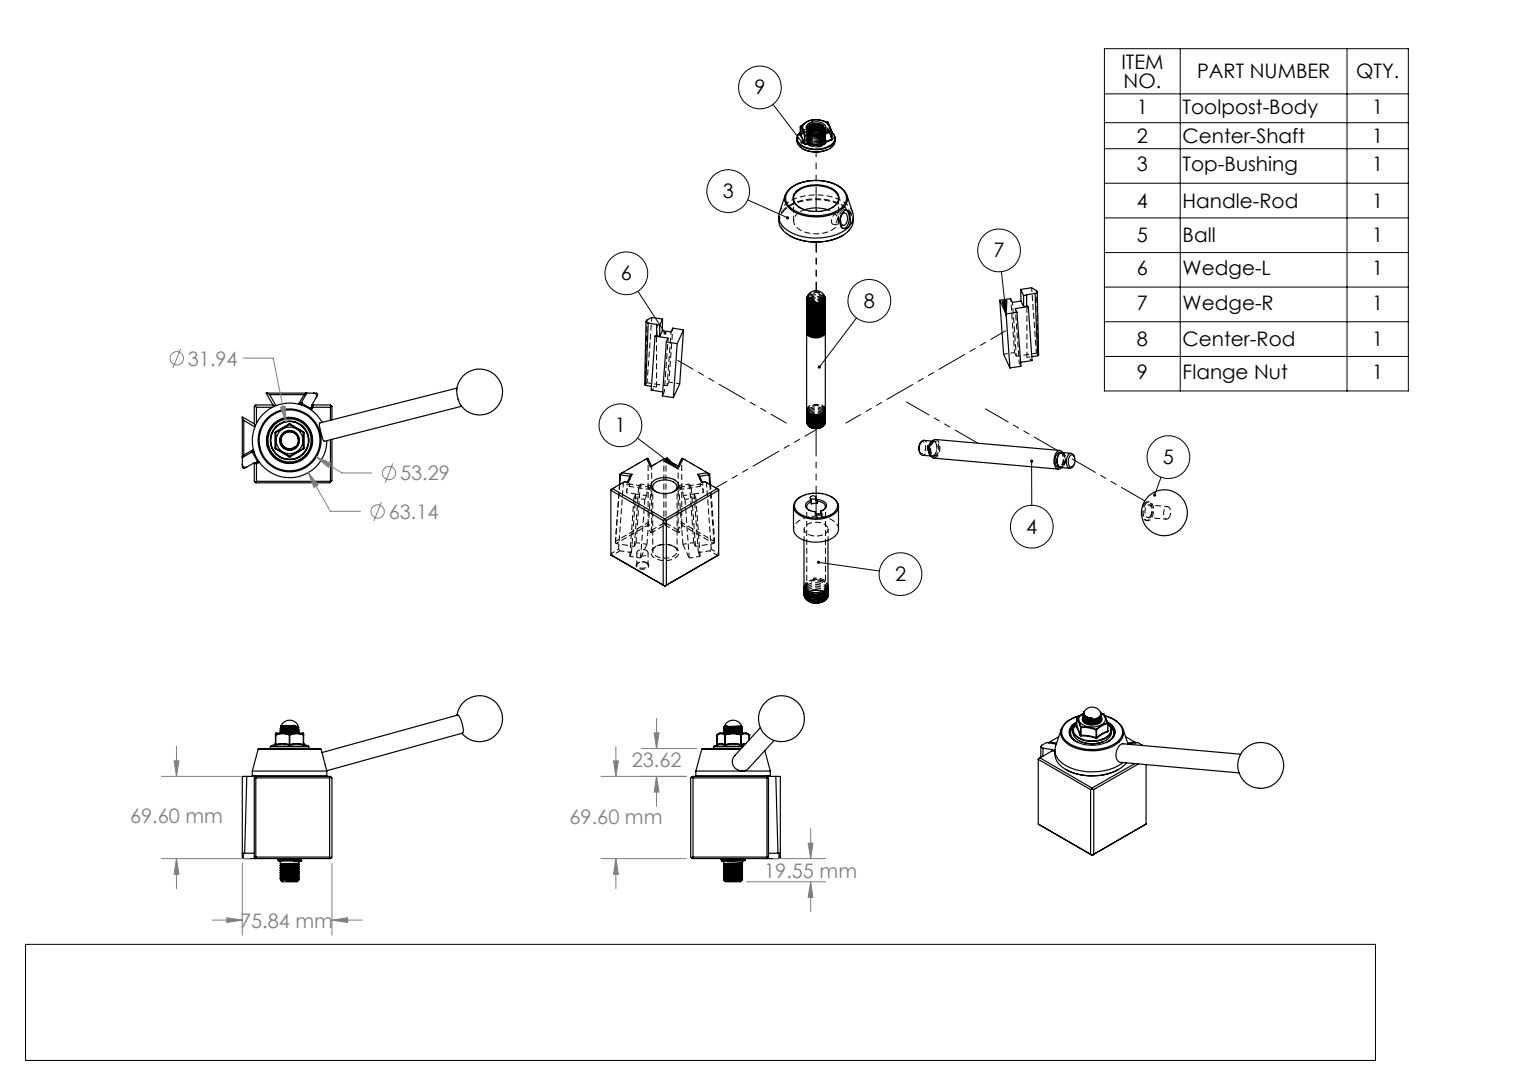
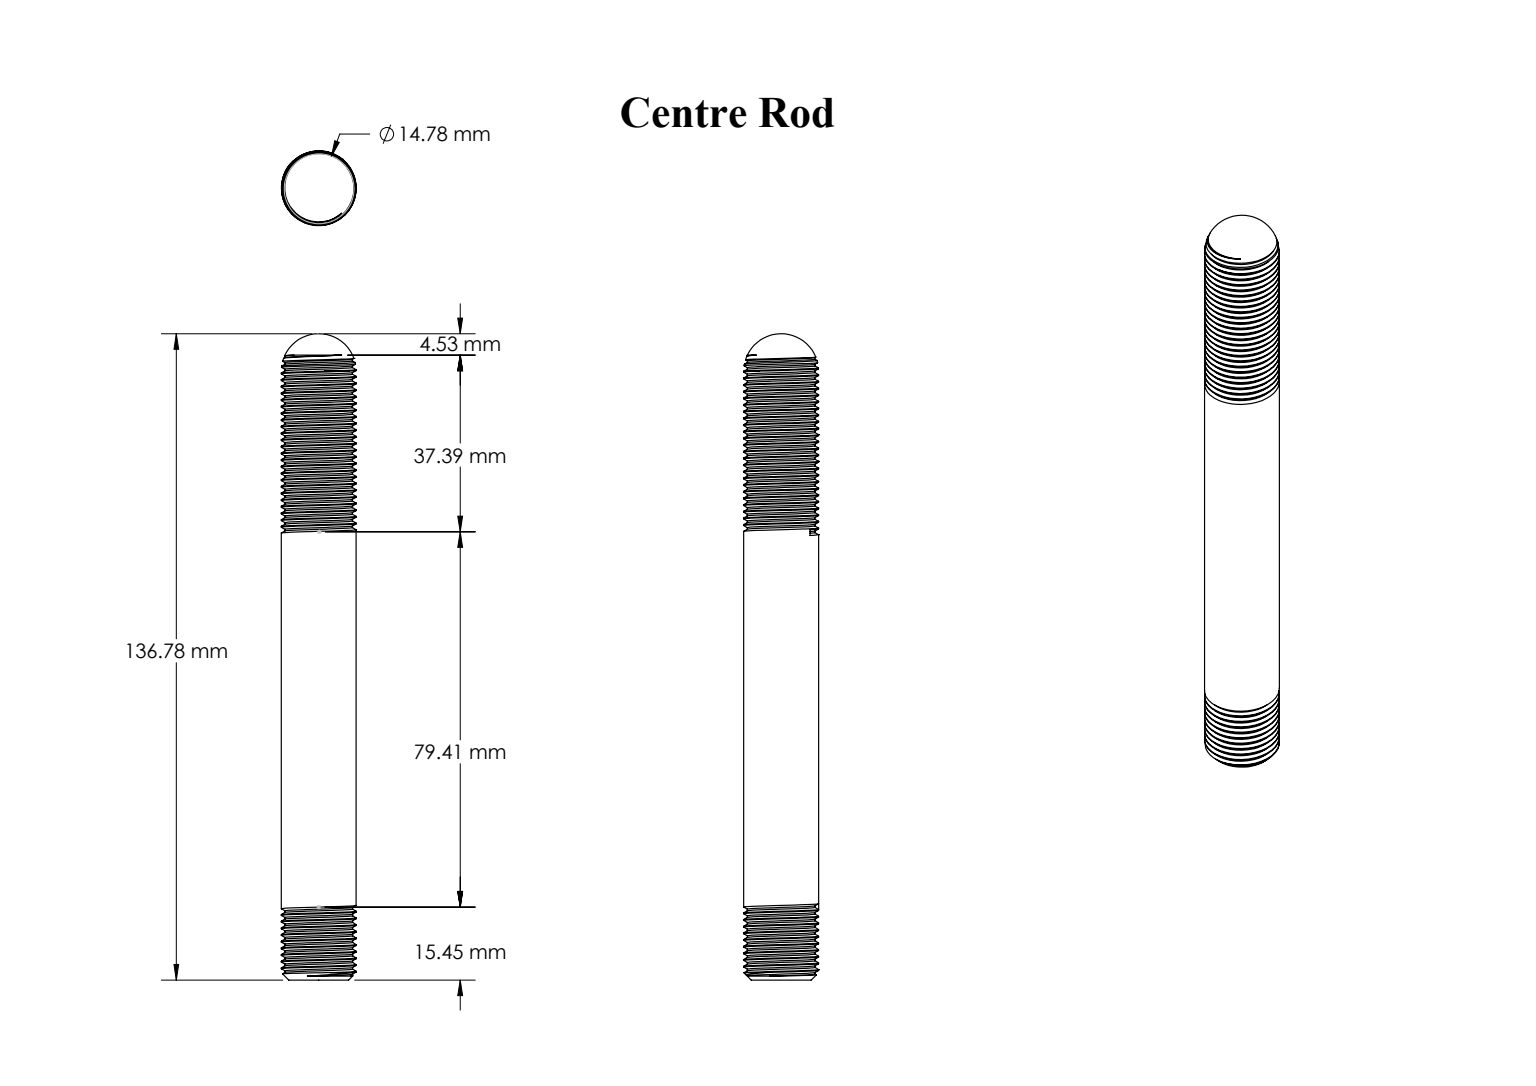
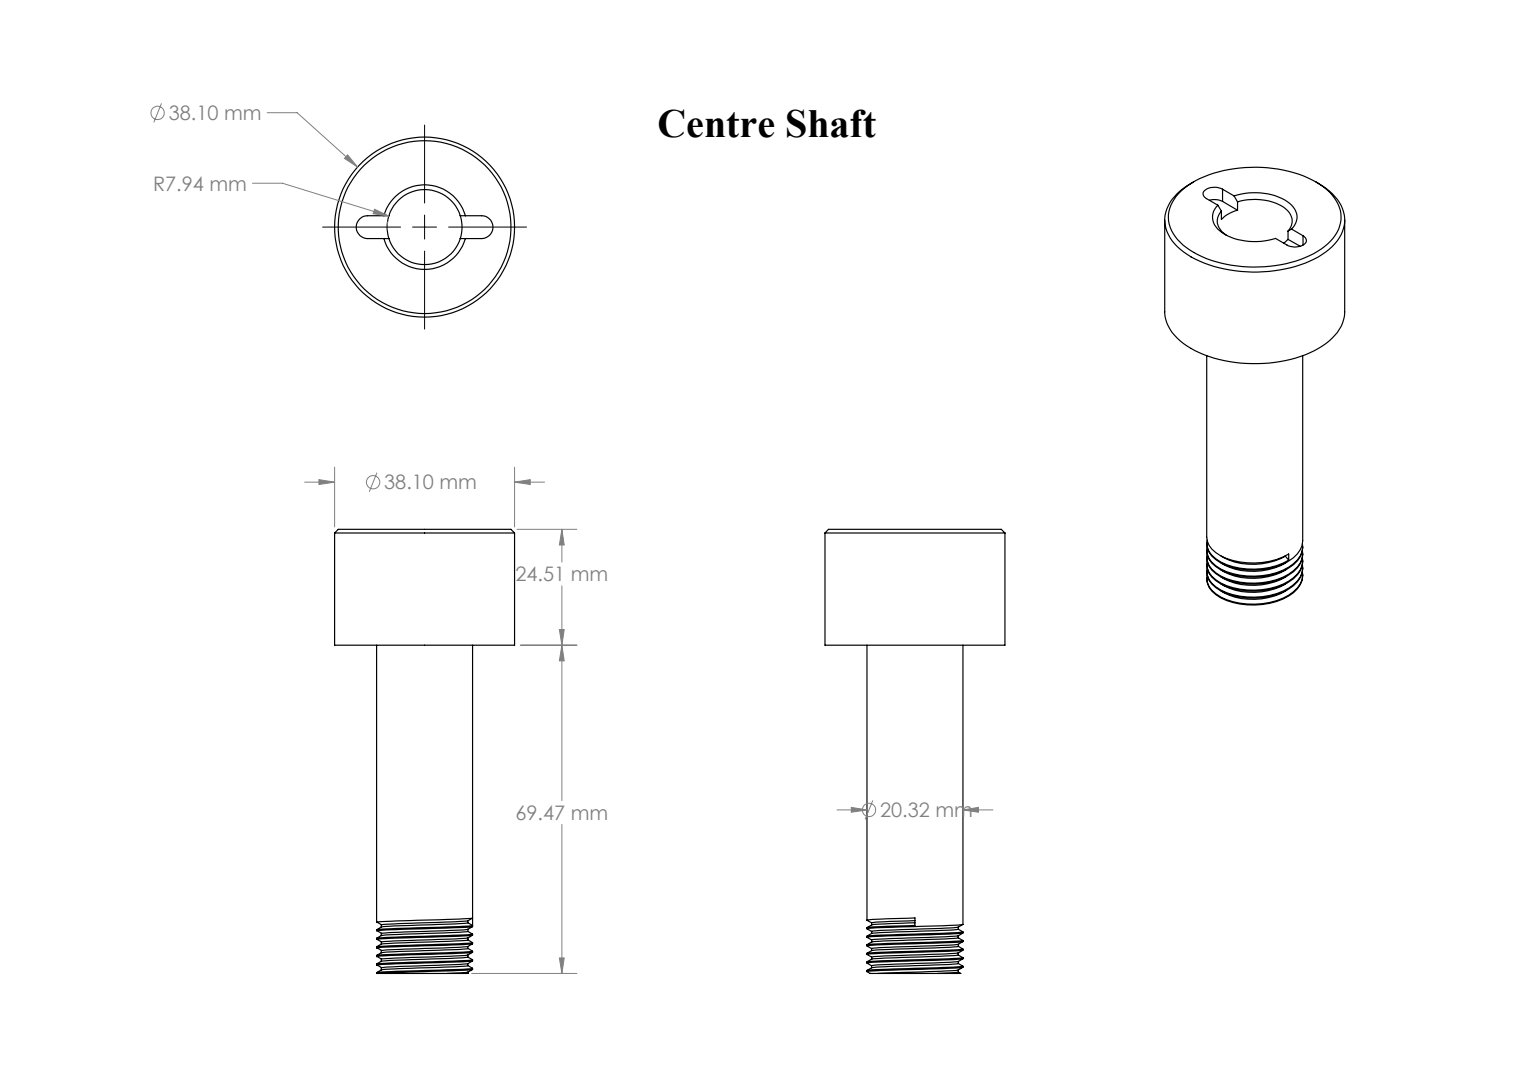
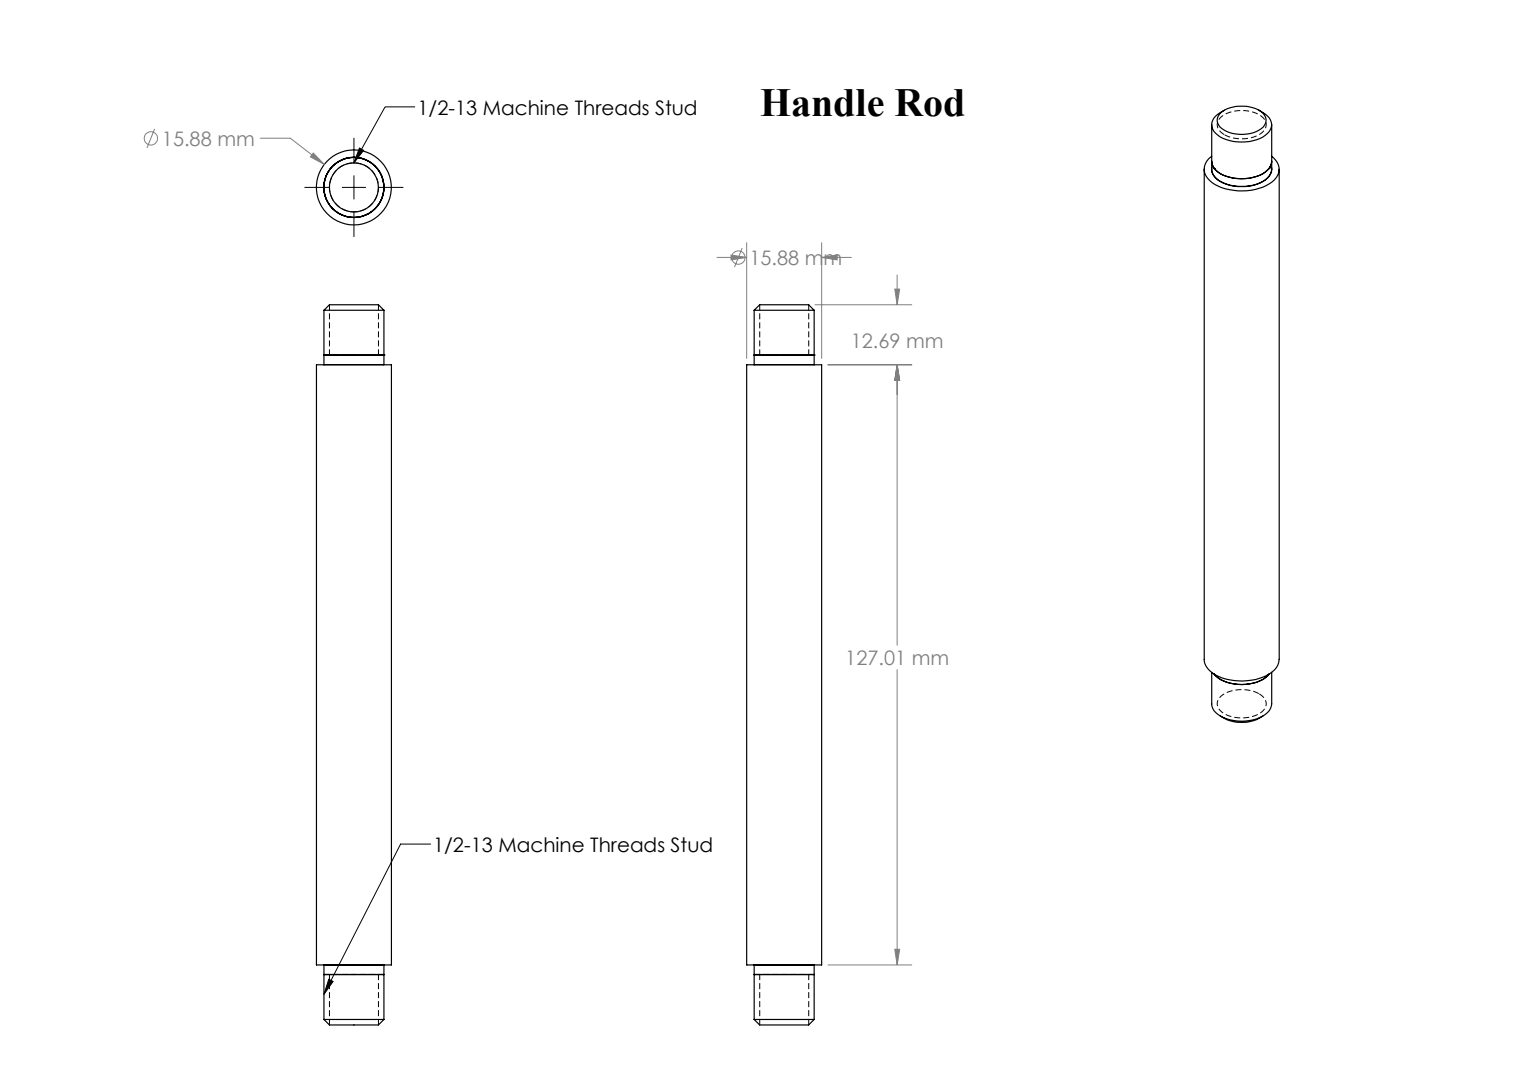
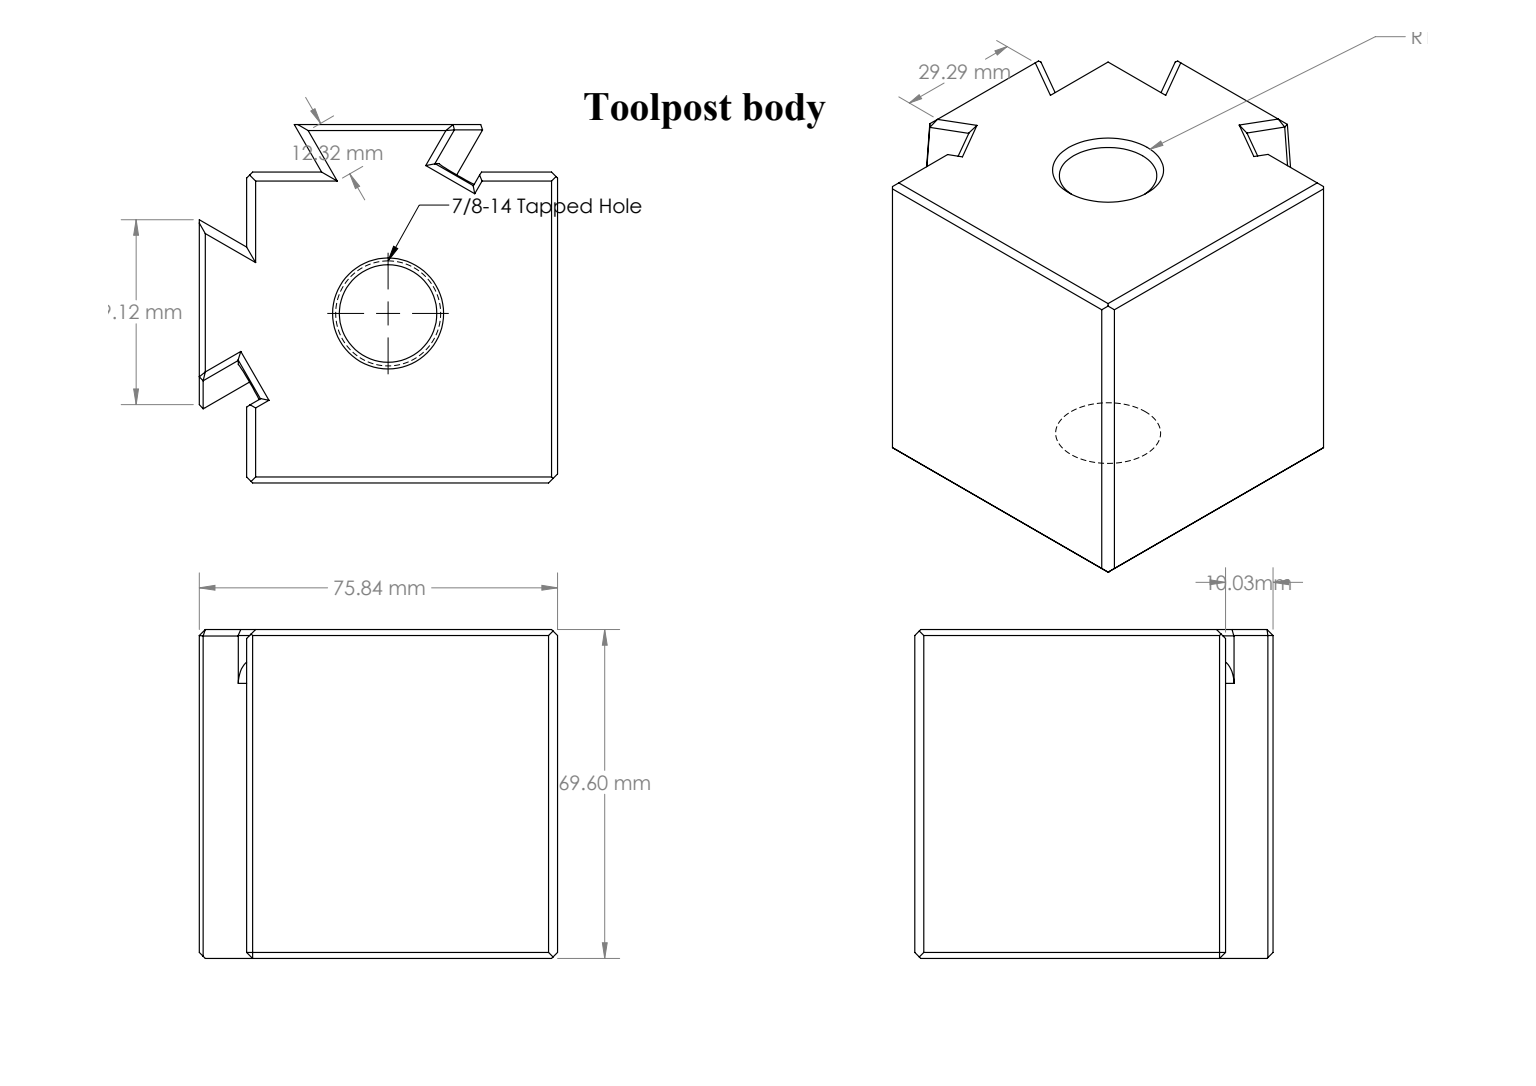
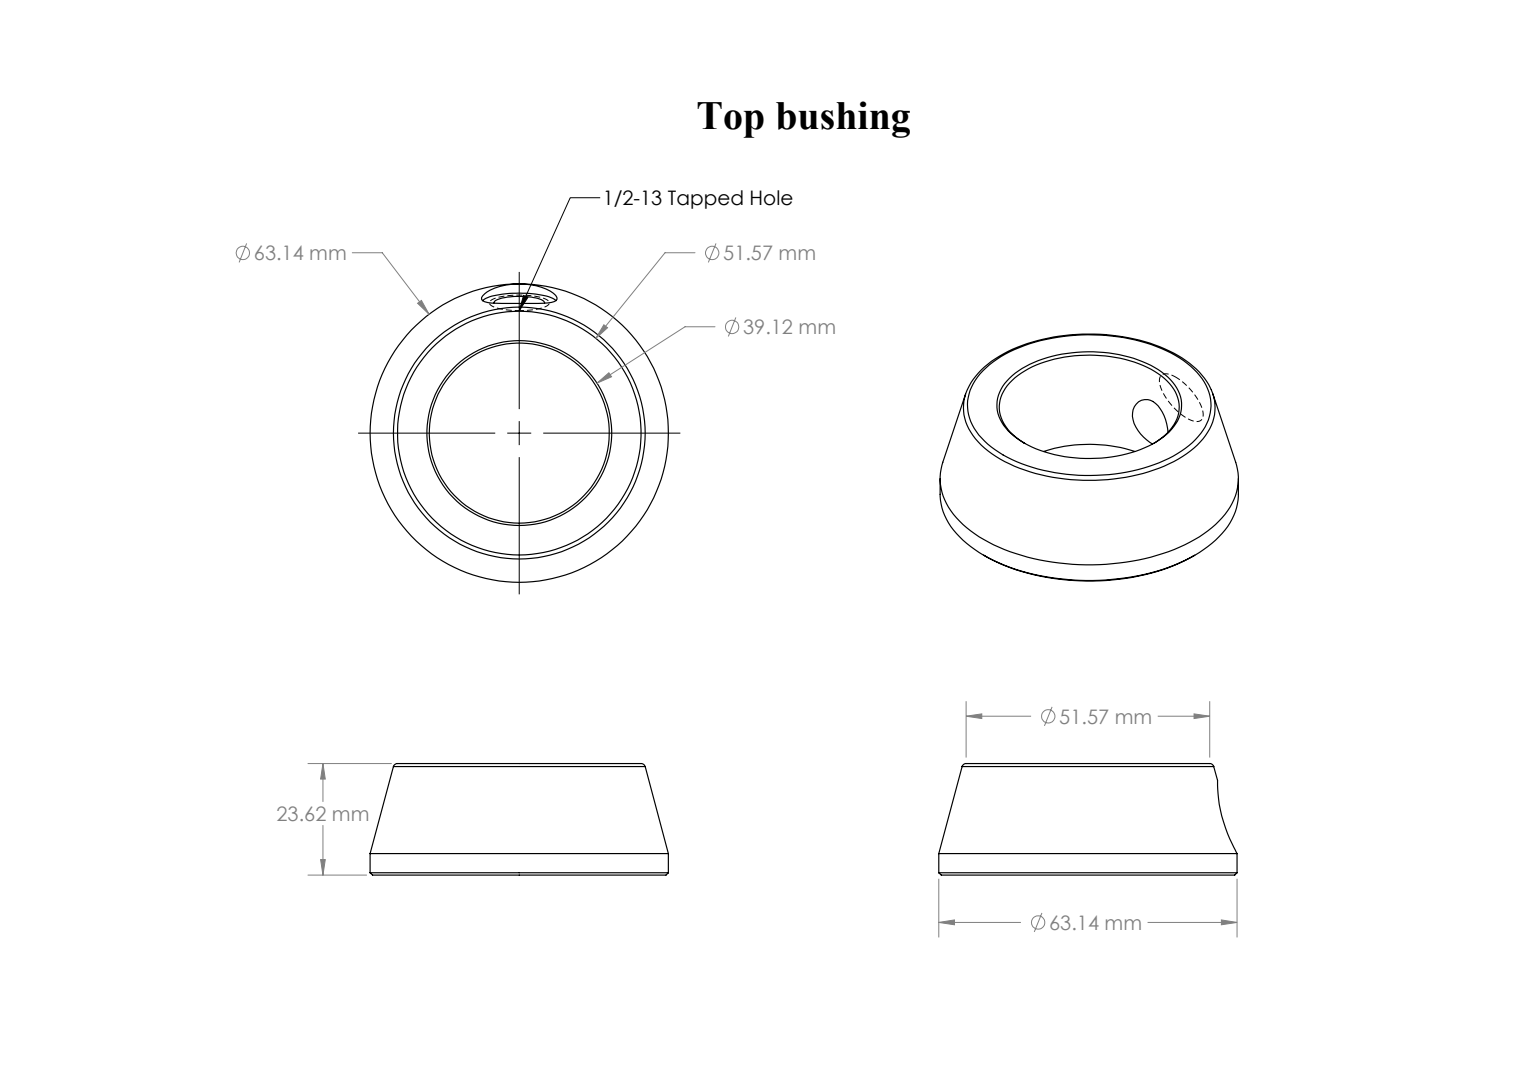
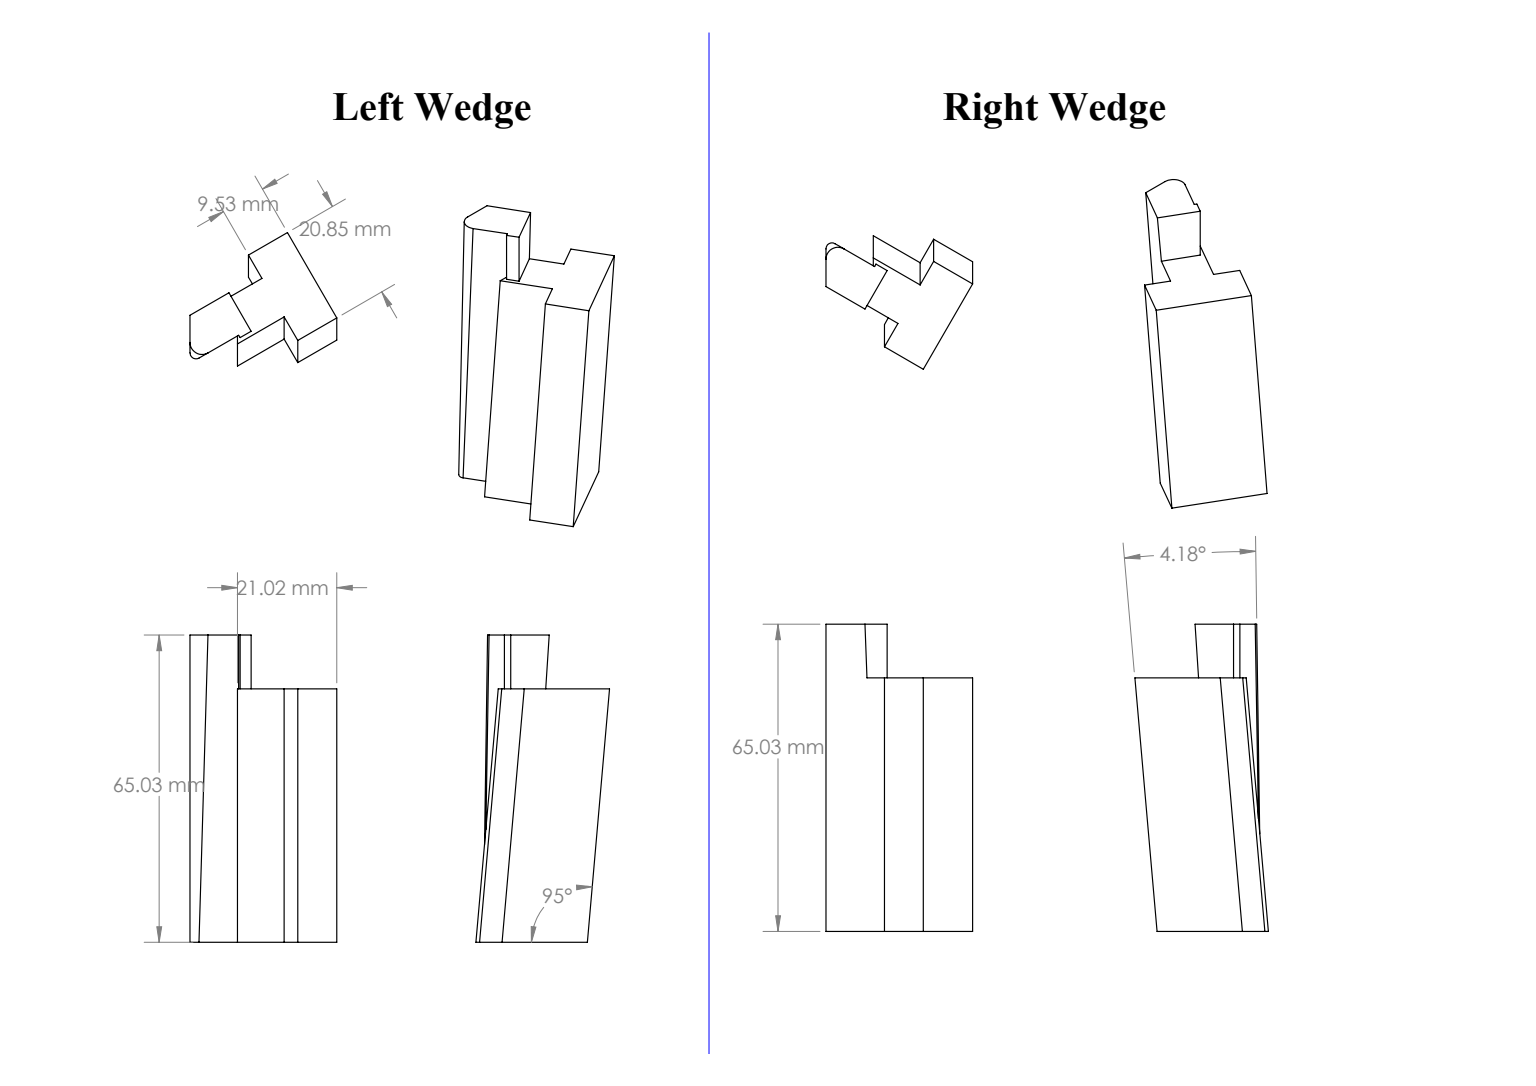
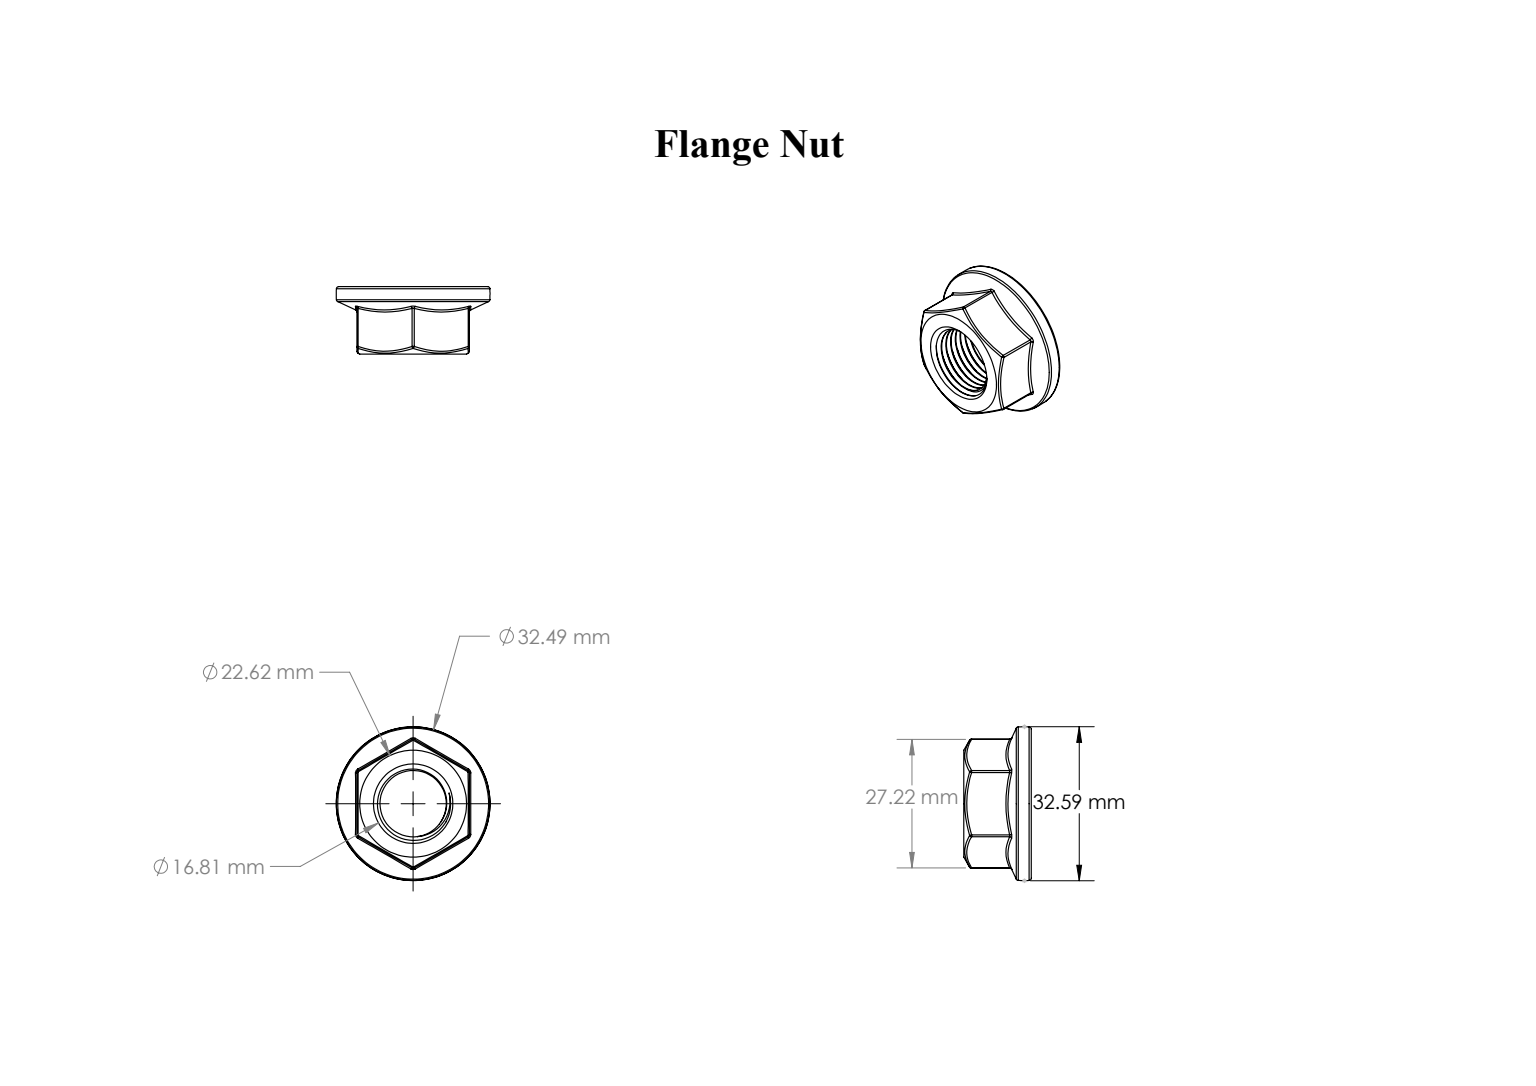
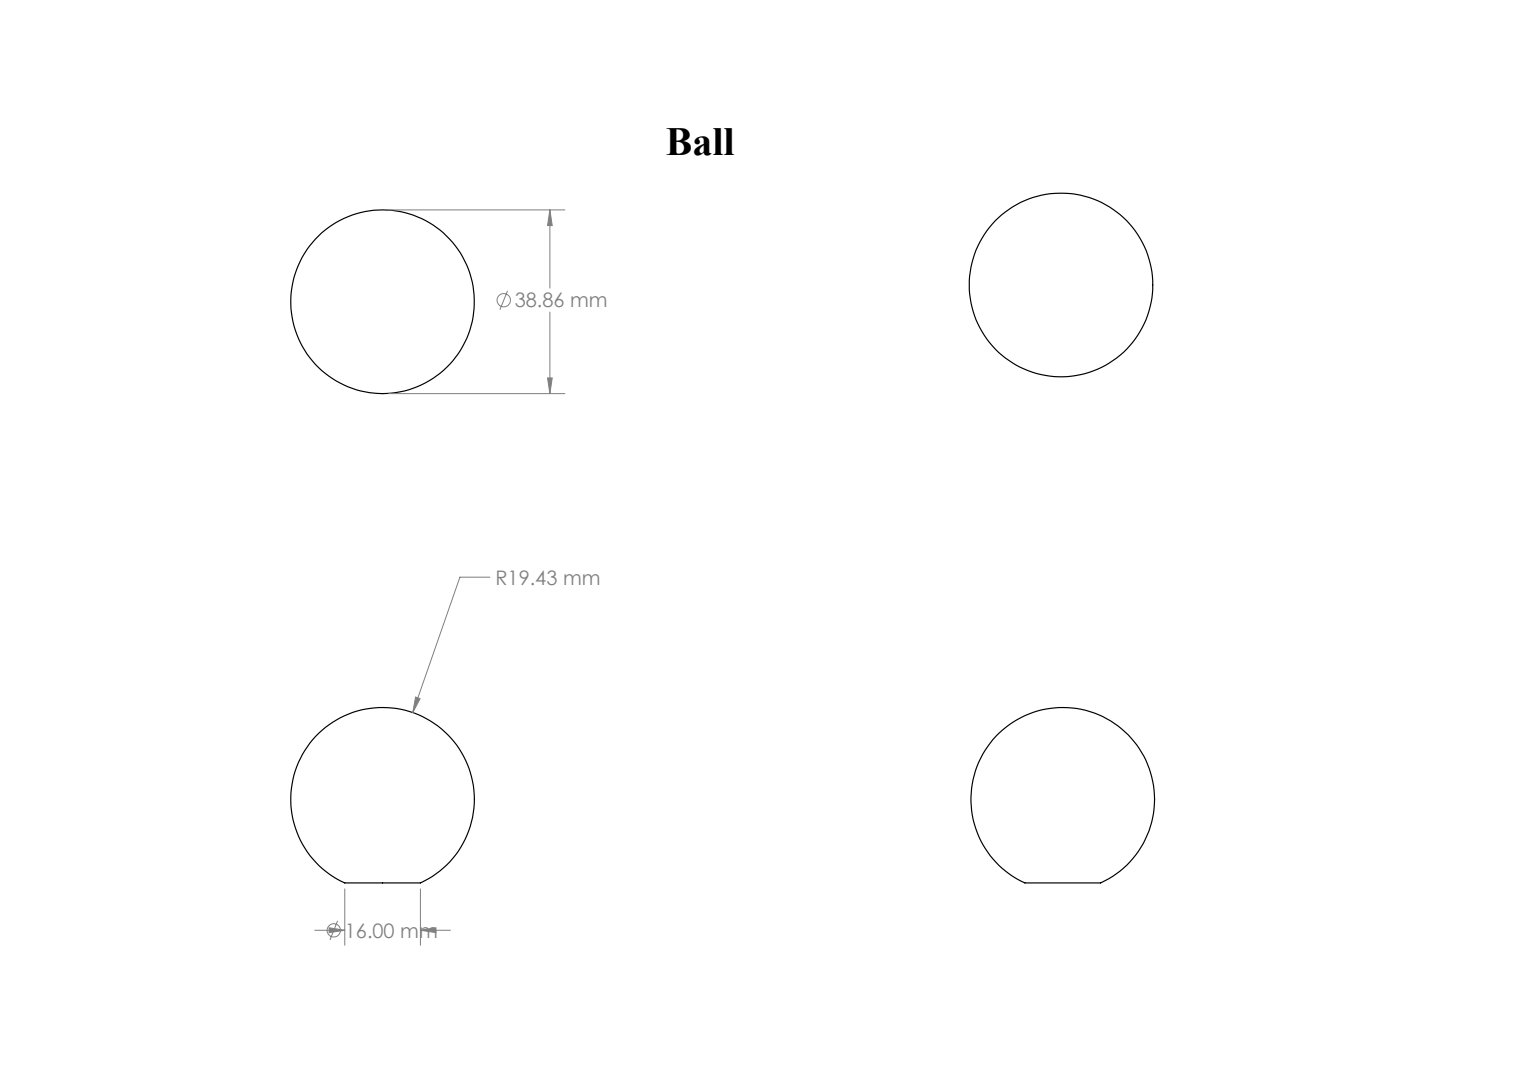
ISO-10303-21;
HEADER;
FILE_DESCRIPTION (('STEP AP203'),
    '1' );
FILE_NAME ('MAS-409',
    '2026-10-07T20:09:13',
    ( '' ),
    ( '' ),
    'SwSTEP 2.0',
    'SolidWorks 2024',
    '' );
FILE_SCHEMA (( 'AUTOMOTIVE_DESIGN' ));
ENDSEC;

DATA;
#1 = DIRECTION ( 'NONE',  ( 1.000000000000000000, 7.888609052210118054E-31, 7.888609052210118054E-31 ) ) ;
#2 = CARTESIAN_POINT ( 'NONE',  ( 0.2472135954999579721, 0.2589285712334865597, -0.3402603233408160732 ) ) ;
#3 = CARTESIAN_POINT ( 'NONE',  ( 1.910449006669871087E-17, 0.1986111111111107386, -0.3119999999999999996 ) ) ;
#4 = CARTESIAN_POINT ( 'NONE',  ( 0.1993543840281267465, 4.595916666742532186, 0.1993543840281266633 ) ) ;
#5 = DATE_AND_TIME ( #15379, #11143 ) ;
#6 = CARTESIAN_POINT ( 'NONE',  ( -0.3119999999999999996, 4.772999999999998799, 0.000000000000000000 ) ) ;
#7 = CARTESIAN_POINT ( 'NONE',  ( 0.8119709581221709049, 2.978485840173427324, -1.588368860739399313 ) ) ;
#8 = CARTESIAN_POINT ( 'NONE',  ( -0.1167790944451422702, 0.4555555554796890116, -0.2819296736111110424 ) ) ;
#9 = ORIENTED_EDGE ( 'NONE', *, *, #4852, .T. ) ;
#10 = EDGE_LOOP ( 'NONE', ( #22952, #23835 ) ) ;
#11 = CARTESIAN_POINT ( 'NONE',  ( -0.1993543840281266633, 0.1256944443685777957, -0.1993543840281266910 ) ) ;
#12 = CARTESIAN_POINT ( 'NONE',  ( 0.4200000000000001510, 0.05000000000000028727, -2.565999999999999837 ) ) ;
#13 = CARTESIAN_POINT ( 'NONE',  ( 0.000000000000000000, 5.384999999999999787, 0.000000000000000000 ) ) ;
#14 = CARTESIAN_POINT ( 'NONE',  ( -0.3236067977499789694, 0.1428571428571428215, -0.2351141009169893104 ) ) ;
#15 = CARTESIAN_POINT ( 'NONE',  ( 0.3155070326520292845, -5.795770164686806123E-17, 0.03451388888889012074 ) ) ;
#16 = CARTESIAN_POINT ( 'NONE',  ( 0.3124999999999999445, -0.1294417382415923856, 0.03625000000000165590 ) ) ;
#17 = AXIS2_PLACEMENT_3D ( 'NONE', #19179, #8074, #22716 ) ;
#18 = FACE_OUTER_BOUND ( 'NONE', #649, .T. ) ;
#19 = CARTESIAN_POINT ( 'NONE',  ( -0.1167790944451422702, 0.2194444443685778234, -0.2819296736111110979 ) ) ;
#20 = CARTESIAN_POINT ( 'NONE',  ( 0.1993543840281266355, 0.02847222214635558926, 0.1993543840281267465 ) ) ;
#21 = VECTOR ( 'NONE', #10740, 39.37007874015748143 ) ;
#22 = CARTESIAN_POINT ( 'NONE',  ( -1.726321361862525858E-17, 4.575083333409199149, -0.2819296736111110979 ) ) ;
#23 = CARTESIAN_POINT ( 'NONE',  ( -0.4000000000000000222, 0.06964285694777234970, -4.898587196589413075E-17 ) ) ;
#24 = CARTESIAN_POINT ( 'NONE',  ( 0.1554777997599670336, -3.800488706749824749E-17, -0.3394405886668848682 ) ) ;
#25 = CARTESIAN_POINT ( 'NONE',  ( 0.1993543840281266633, 5.179250000075866112, -0.1993543840281266910 ) ) ;
#26 = CARTESIAN_POINT ( 'NONE',  ( -0.2819296736111110979, 4.349388888964754507, -0.1167790944451422980 ) ) ;
#27 = CARTESIAN_POINT ( 'NONE',  ( 0.3137165877996647145, 3.752159157235426701, 0.001669988021508127815 ) ) ;
#28 = CARTESIAN_POINT ( 'NONE',  ( -0.1899274842524383000, 0.4207833852643000361, 0.4343212420608417168 ) ) ;
#29 = DIRECTION ( 'NONE',  ( -0.000000000000000000, -1.000000000000000000, -0.000000000000000000 ) ) ;
#30 = ADVANCED_FACE ( 'NONE', ( #19654 ), #17708, .T. ) ;
#31 = CARTESIAN_POINT ( 'NONE',  ( -0.1292346314604057023, 4.123694444596177178, 0.3119999999999998885 ) ) ;
#32 = CARTESIAN_POINT ( 'NONE',  ( -0.2819296736111110979, 4.533416666742532186, 0.000000000000000000 ) ) ;
#33 = DIRECTION ( 'NONE',  ( 0.000000000000000000, 0.7071067811865497932, 0.7071067811865452413 ) ) ;
#34 = EDGE_CURVE ( 'NONE', #12593, #3702, #6524, .T. ) ;
#35 = CARTESIAN_POINT ( 'NONE',  ( -0.3616234456863465230, 3.514980167629567998, 2.635972749958888528 ) ) ;
#36 = ORIENTED_EDGE ( 'NONE', *, *, #677, .F. ) ;
#37 = VECTOR ( 'NONE', #16324, 39.37007874015748143 ) ;
#38 = ORIENTED_EDGE ( 'NONE', *, *, #20394, .F. ) ;
#39 = PERSON_AND_ORGANIZATION_ROLE ( 'classification_officer' ) ;
#40 = FACE_OUTER_BOUND ( 'NONE', #1469, .T. ) ;
#41 = CARTESIAN_POINT ( 'NONE',  ( 0.4208308994021709992, -0.2864083541825031554, 0.4065068718547069082 ) ) ;
#42 = DIRECTION ( 'NONE',  ( -0.000000000000000000, 0.000000000000000000, 1.000000000000000000 ) ) ;
#43 = EDGE_LOOP ( 'NONE', ( #17199, #17644, #7483, #15061 ) ) ;
#44 = CARTESIAN_POINT ( 'NONE',  ( -0.3119999999999999996, 0.4277777776260448528, -3.820898013339742174E-17 ) ) ;
#45 = VERTEX_POINT ( 'NONE', #6974 ) ;
#46 = DIRECTION ( 'NONE',  ( 0.000000000000000000, 0.000000000000000000, -1.000000000000000000 ) ) ;
#47 = CARTESIAN_POINT ( 'NONE',  ( -0.3140464948364212194, 3.723602166599303764, -0.02909203108594766995 ) ) ;
#48 = CARTESIAN_POINT ( 'NONE',  ( -0.1116596296178200276, 0.04374999990245760639, 0.3436530038418508792 ) ) ;
#49 = CARTESIAN_POINT ( 'NONE',  ( 0.1916168258699956772, 3.966268988801258555, 0.2495847059250467792 ) ) ;
#50 = ORIENTED_EDGE ( 'NONE', *, *, #21102, .T. ) ;
#51 = CARTESIAN_POINT ( 'NONE',  ( 0.3613381517857143232, 0.08660714275960043618, -0.1174058825155740587 ) ) ;
#52 = ORIENTED_EDGE ( 'NONE', *, *, #22032, .T. ) ;
#53 = CARTESIAN_POINT ( 'NONE',  ( 0.4500000000000003442, 0.2598076211353318454, 0.3779506566538942125 ) ) ;
#54 = CARTESIAN_POINT ( 'NONE',  ( -0.2764156081756484196, 1.692557448933383907E-17, 0.2550000000000032241 ) ) ;
#55 = CARTESIAN_POINT ( 'NONE',  ( 0.1167790944451422702, 4.279944444520310753, -0.2819296736111110424 ) ) ;
#56 = CARTESIAN_POINT ( 'NONE',  ( 5.178964085587577574E-17, 5.033416666742532186, 0.2819296736111110979 ) ) ;
#57 = CARTESIAN_POINT ( 'NONE',  ( -0.1504789989860494670, -0.4433647533406467889, 0.4295860435587943171 ) ) ;
#58 = CARTESIAN_POINT ( 'NONE',  ( -0.3886629897678103851, 0.3298823763122804564, 0.06108558933789665774 ) ) ;
#59 = EDGE_CURVE ( 'NONE', #5903, #21880, #9041, .T. ) ;
#60 = CARTESIAN_POINT ( 'NONE',  ( -0.1292346314604057023, 3.894527777777776478, 0.3119999999999998885 ) ) ;
#61 = EDGE_CURVE ( 'NONE', #19679, #20558, #12738, .T. ) ;
#62 = ADVANCED_FACE ( 'NONE', ( #18066 ), #7215, .T. ) ;
#63 = CARTESIAN_POINT ( 'NONE',  ( 0.1292346314604056190, 4.707027777929510215, -0.3119999999999999996 ) ) ;
#64 = CARTESIAN_POINT ( 'NONE',  ( 0.1337853507730711877, 4.797771151123610522, 0.2837542960833542294 ) ) ;
#65 = CARTESIAN_POINT ( 'NONE',  ( 0.2206173157302028232, 0.4138888888888885287, -0.2206173157302028232 ) ) ;
#66 = EDGE_LOOP ( 'NONE', ( #14998, #20561, #21029, #16643 ) ) ;
#67 = CARTESIAN_POINT ( 'NONE',  ( 0.2923287055106771337, 0.2008928570453147044, 0.2123892367102621359 ) ) ;
#68 = EDGE_CURVE ( 'NONE', #2537, #6211, #23657, .T. ) ;
#69 = CARTESIAN_POINT ( 'NONE',  ( 2.055580586463031434, 2.740000000000000213, -2.936000000000001720 ) ) ;
#70 = VERTEX_POINT ( 'NONE', #16487 ) ;
#71 = PERSON_AND_ORGANIZATION ( #15518, #2538 ) ;
#72 = DIRECTION ( 'NONE',  ( 0.000000000000000000, 0.000000000000000000, 1.000000000000000000 ) ) ;
#73 = CARTESIAN_POINT ( 'NONE',  ( -0.2819296736111110424, 5.134111111186975940, 0.1167790944451424923 ) ) ;
#74 = CARTESIAN_POINT ( 'NONE',  ( -0.2819296736111110979, 3.866750000075866112, 0.000000000000000000 ) ) ;
#75 = CARTESIAN_POINT ( 'NONE',  ( 0.2732891327808320558, -0.3834823229876774264, 0.4280258002685559671 ) ) ;
#76 = CARTESIAN_POINT ( 'NONE',  ( -0.4316174467094854306, 0.9548081934128058723, 2.771794876808019836 ) ) ;
#77 = EDGE_LOOP ( 'NONE', ( #1888, #18822, #18555, #19530 ) ) ;
#78 = CARTESIAN_POINT ( 'NONE',  ( -0.2764156081756484196, 1.692557448933383907E-17, 0.08833333333333522053 ) ) ;
#79 = CARTESIAN_POINT ( 'NONE',  ( 0.1993543840281266910, 0.1673611110352444808, -0.1993543840281266910 ) ) ;
#80 = CARTESIAN_POINT ( 'NONE',  ( 0.1144950937579609085, -0.2764156081756484751, 0.2793055555555589153 ) ) ;
#81 = CARTESIAN_POINT ( 'NONE',  ( -0.1167790944451423257, 5.023000000075867000, -0.2819296736111110424 ) ) ;
#82 = CARTESIAN_POINT ( 'NONE',  ( 0.1572276619573833301, 4.465128489813300128, 0.2725687012519474872 ) ) ;
#83 = CARTESIAN_POINT ( 'NONE',  ( -0.2819296736111110424, 4.960500000075865223, -0.1167790944451423119 ) ) ;
#84 = CARTESIAN_POINT ( 'NONE',  ( 0.3950000000000000178, 2.740039370078740433, -1.966000000000000192 ) ) ;
#85 = EDGE_CURVE ( 'NONE', #8682, #18897, #14418, .T. ) ;
#86 = LINE ( 'NONE', #23728, #15966 ) ;
#87 = DIRECTION ( 'NONE',  ( 0.000000000000000000, 0.000000000000000000, -1.000000000000000000 ) ) ;
#88 = CARTESIAN_POINT ( 'NONE',  ( 0.2206173157302028787, 4.460499999999998799, 0.2206173157302027954 ) ) ;
#89 = EDGE_CURVE ( 'NONE', #12827, #10130, #5133, .T. ) ;
#90 = CARTESIAN_POINT ( 'NONE',  ( 0.2819296736111110979, 3.773000000075866112, -0.1167790944451423396 ) ) ;
#91 = LINE ( 'NONE', #7534, #15165 ) ;
#92 = CARTESIAN_POINT ( 'NONE',  ( 0.01188239640610571149, 4.043514080066898053, -0.3119999715909181903 ) ) ;
#93 = CARTESIAN_POINT ( 'NONE',  ( -0.01999320810728339587, 3.737730494582271579, 0.3119999990119339817 ) ) ;
#94 = ORIENTED_EDGE ( 'NONE', *, *, #21035, .F. ) ;
#95 = DIRECTION ( 'NONE',  ( -0.4995222938423184988, -0.04370253788966844966, 0.8651979924482664508 ) ) ;
#96 = ORIENTED_EDGE ( 'NONE', *, *, #12472, .T. ) ;
#97 = EDGE_CURVE ( 'NONE', #19422, #8315, #12597, .T. ) ;
#98 = CARTESIAN_POINT ( 'NONE',  ( -0.009374999999999907713, -0.5358532185916218271, 0.3779506566538943235 ) ) ;
#99 = AXIS2_PLACEMENT_3D ( 'NONE', #2316, #21202, #17426 ) ;
#100 = CARTESIAN_POINT ( 'NONE',  ( 0.3125000000000000000, 3.827021247335477694E-17, 1.326383476483184332 ) ) ;
#101 =( BOUNDED_CURVE ( )  B_SPLINE_CURVE ( 2, ( #22373, #3964, #5909, #11408, #18841, #2137, #22623, #13366, #20787 ),
 .UNSPECIFIED., .F., .F. ) 
 B_SPLINE_CURVE_WITH_KNOTS ( ( 3, 2, 2, 2, 3 ),
 ( 0.2767857142857141350, 0.2812499999999998335, 0.2857142857142855319, 0.2901785714285712858, 0.2946428571428569843 ),
 .UNSPECIFIED. ) 
 CURVE ( )  GEOMETRIC_REPRESENTATION_ITEM ( )  RATIONAL_B_SPLINE_CURVE ( ( 1.000000000000002887, 0.9238795325112838519, 1.000000000000000000, 0.9238795325112867385, 1.000000000000000000, 0.9238795325112867385, 1.000000000000000000, 0.9238795325112896251, 0.9999999999999971134 ) ) 
 REPRESENTATION_ITEM ( '' )  );
#102 = CARTESIAN_POINT ( 'NONE',  ( -3.385114897866767815E-17, -0.2764156081756484196, 0.2133333333333362336 ) ) ;
#103 = CARTESIAN_POINT ( 'NONE',  ( -0.1292346314604058410, 0.3895833333333330040, 0.3119999999999998885 ) ) ;
#104 = CARTESIAN_POINT ( 'NONE',  ( 0.000000000000000000, 5.501232050807569607, 0.000000000000000000 ) ) ;
#105 = ORIENTED_EDGE ( 'NONE', *, *, #5573, .F. ) ;
#106 = CARTESIAN_POINT ( 'NONE',  ( 0.3613381517857143232, 0.3723214284738861068, -0.1174058825155740587 ) ) ;
#107 = CARTESIAN_POINT ( 'NONE',  ( 1.726321361862525858E-17, 0.3270833332574666907, -0.2819296736111110979 ) ) ;
#108 = CARTESIAN_POINT ( 'NONE',  ( 0.4687500000000002776, -0.2172231356220941378, 0.07046374828496694553 ) ) ;
#109 = CARTESIAN_POINT ( 'NONE',  ( 0.3129697935626465366, 0.5133535954949590696, -1.110419158421684260 ) ) ;
#110 = CARTESIAN_POINT ( 'NONE',  ( -0.3119999999999999996, 0.1569444444444440812, -3.820898013339742174E-17 ) ) ;
#111 = CARTESIAN_POINT ( 'NONE',  ( 0.2764156081756483641, -0.1144950937579611167, -0.04708333333333256793 ) ) ;
#112 = EDGE_LOOP ( 'NONE', ( #9913, #3246, #2144, #17616 ) ) ;
#113 = LINE ( 'NONE', #7555, #14963 ) ;
#114 = CARTESIAN_POINT ( 'NONE',  ( 0.4687500000000003331, -0.1769877694293681969, 0.4113775649628997333 ) ) ;
#115 = CARTESIAN_POINT ( 'NONE',  ( -0.3119999999999999996, 0.1013888888888885564, -3.820898013339742174E-17 ) ) ;
#116 = CARTESIAN_POINT ( 'NONE',  ( -0.1292346314604057023, 5.061194444444443441, 0.3119999999999998885 ) ) ;
#117 = CARTESIAN_POINT ( 'NONE',  ( -0.2923287055106771337, 0.2687499999024575703, 0.2123892367102619971 ) ) ;
#118 = VECTOR ( 'NONE', #23345, 39.37007874015748143 ) ;
#119 = CARTESIAN_POINT ( 'NONE',  ( -0.1167790944451423535, 4.210500000075866112, 0.2819296736111110424 ) ) ;
#120 = CARTESIAN_POINT ( 'NONE',  ( 0.3119999999999998885, 0.1187499998482670627, 0.1292346314604058410 ) ) ;
#121 = CARTESIAN_POINT ( 'NONE',  ( 0.3587893197688488689, 1.447158556123030749E-17, -0.04444430867843930655 ) ) ;
#122 = ORIENTED_EDGE ( 'NONE', *, *, #2601, .F. ) ;
#123 = CARTESIAN_POINT ( 'NONE',  ( -0.4719654084974831409, -0.2800274776536547106, 0.04212966708837322799 ) ) ;
#124 = EDGE_CURVE ( 'NONE', #17018, #2833, #252, .T. ) ;
#125 = CARTESIAN_POINT ( 'NONE',  ( -0.1167790944451423257, 5.009111111186976828, -0.2819296736111110424 ) ) ;
#126 = ADVANCED_FACE ( 'NONE', ( #2334 ), #2953, .F. ) ;
#127 = DIRECTION ( 'NONE',  ( -0.6125180959723208751, -0.6125180959723208751, 0.4996430367901520953 ) ) ;
#128 =( NAMED_UNIT ( * ) PLANE_ANGLE_UNIT ( ) SI_UNIT ( $, .RADIAN. ) );
#129 = CARTESIAN_POINT ( 'NONE',  ( 0.001964067453944123073, 3.710447205286024897, -0.3119947023668593333 ) ) ;
#130 = DIRECTION ( 'NONE',  ( 0.000000000000000000, 0.000000000000000000, -1.000000000000000000 ) ) ;
#131 = CARTESIAN_POINT ( 'NONE',  ( 0.1167790944451422702, 4.613277777853643791, -0.2819296736111110979 ) ) ;
#132 = CONTEXT_DEPENDENT_SHAPE_REPRESENTATION ( #13424, #9353 ) ;
#133 = PLANE ( 'NONE',  #11743 ) ;
#134 = FACE_OUTER_BOUND ( 'NONE', #4569, .T. ) ;
#135 = CARTESIAN_POINT ( 'NONE',  ( -0.2819296736111110979, 0.4138888888130222155, 0.1167790944451422425 ) ) ;
#136 = ORIENTED_EDGE ( 'NONE', *, *, #22688, .T. ) ;
#137 = CARTESIAN_POINT ( 'NONE',  ( 0.2819296736111110979, 0.2715277777019111660, 0.000000000000000000 ) ) ;
#138 = CARTESIAN_POINT ( 'NONE',  ( -0.1797761229313996068, 4.715880237781718165, -0.2556404866186153257 ) ) ;
#139 = DIRECTION ( 'NONE',  ( 0.000000000000000000, -1.000000000000000000, -0.000000000000000000 ) ) ;
#140 = CARTESIAN_POINT ( 'NONE',  ( 0.4000000000000000222, 0.1142857142857142405, 0.000000000000000000 ) ) ;
#141 = CARTESIAN_POINT ( 'NONE',  ( -0.1306872919485614903, 0.3155070326520293400, 0.05187500000000137834 ) ) ;
#142 = CARTESIAN_POINT ( 'NONE',  ( -0.009374999999999892100, -0.5358532185916218271, 0.06112444011295370405 ) ) ;
#143 = DIRECTION ( 'NONE',  ( 0.7071067811865475727, -0.7071067811865475727, 0.000000000000000000 ) ) ;
#144 = CARTESIAN_POINT ( 'NONE',  ( 1.726321361862525858E-17, 0.3270833332574666907, -0.2819296736111110979 ) ) ;
#145 = CARTESIAN_POINT ( 'NONE',  ( 0.9995881047227681560, 2.471730513698206178, -1.219071084208098732 ) ) ;
#146 = CARTESIAN_POINT ( 'NONE',  ( 0.1167790944451422702, 4.293833333409199149, -0.2819296736111110424 ) ) ;
#147 = CARTESIAN_POINT ( 'NONE',  ( -0.1236067977499789583, 0.1267857140906294977, -0.3804226065180614791 ) ) ;
#148 = CARTESIAN_POINT ( 'NONE',  ( -0.1167790944451423535, 4.766055555631421470, 0.2819296736111110424 ) ) ;
#149 =( BOUNDED_CURVE ( )  B_SPLINE_CURVE ( 2, ( #23578, #18111, #14462, #1644, #20183, #18233, #14334, #18593, #6894 ),
 .UNSPECIFIED., .F., .F. ) 
 B_SPLINE_CURVE_WITH_KNOTS ( ( 3, 2, 2, 2, 3 ),
 ( 0.02744854538997967483, 0.03125000000000000000, 0.04166666666666667823, 0.05208333333333335646, 0.06250000000000002776 ),
 .UNSPECIFIED. ) 
 CURVE ( )  GEOMETRIC_REPRESENTATION_ITEM ( )  RATIONAL_B_SPLINE_CURVE ( ( 0.9647168388458802202, 0.9722206238030204339, 1.000000000000000000, 0.9238795325112867385, 1.000000000000000000, 0.9238795325112867385, 1.000000000000000000, 0.9238795325112865164, 1.000000000000000222 ) ) 
 REPRESENTATION_ITEM ( '' )  );
#150 = PRODUCT_RELATED_PRODUCT_CATEGORY ( 'detail', '', ( #18099 ) ) ;
#151 = CARTESIAN_POINT ( 'NONE',  ( -0.1167790944451423119, 4.453555555631420582, -0.2819296736111110979 ) ) ;
#152 = CARTESIAN_POINT ( 'NONE',  ( 0.3125000000000000000, -5.740531871003217465E-17, 0.3175000000000038347 ) ) ;
#153 = EDGE_LOOP ( 'NONE', ( #3116, #23568, #3841, #12769 ) ) ;
#154 = CARTESIAN_POINT ( 'NONE',  ( -0.07966834441866296745, 4.768317572005395633, -0.3042764398256994629 ) ) ;
#155 = CARTESIAN_POINT ( 'NONE',  ( -1.910449006669871087E-17, 4.154944444596176290, -0.3119999999999999996 ) ) ;
#156 = AXIS2_PLACEMENT_3D ( 'NONE', #2067, #15007, #355 ) ;
#157 = DIRECTION ( 'NONE',  ( 0.000000000000000000, 0.000000000000000000, 1.000000000000000000 ) ) ;
#158 = CARTESIAN_POINT ( 'NONE',  ( 0.05458059743777703143, -0.3010824892324204249, -0.09469801875939774793 ) ) ;
#159 = EDGE_LOOP ( 'NONE', ( #9188, #6198, #17290, #20083, #1245, #14099, #50 ) ) ;
#160 = APPROVAL_ROLE ( '' ) ;
#161 = CARTESIAN_POINT ( 'NONE',  ( -0.3119999999999998885, 4.276472222222222008, 0.1292346314604058410 ) ) ;
#162 = EDGE_LOOP ( 'NONE', ( #18983, #19188, #20187, #19564 ) ) ;
#163 = CARTESIAN_POINT ( 'NONE',  ( -0.1953777901228682112, 4.843409774179208149, 0.2460124067163272643 ) ) ;
#164 = CARTESIAN_POINT ( 'NONE',  ( -1.916134881958141055E-16, 0.5412658773652744282, 0.4425000000000000044 ) ) ;
#165 = EDGE_CURVE ( 'NONE', #15529, #11169, #6067, .T. ) ;
#166 = ORIENTED_EDGE ( 'NONE', *, *, #16153, .T. ) ;
#167 = CARTESIAN_POINT ( 'NONE',  ( 0.2206173157302027676, 0.3930555554038225874, 0.2206173157302028787 ) ) ;
#168 = ORIENTED_EDGE ( 'NONE', *, *, #11879, .F. ) ;
#169 = CARTESIAN_POINT ( 'NONE',  ( 0.4449999999999992850, 0.000000000000000000, -0.4288675134594802096 ) ) ;
#170 = CARTESIAN_POINT ( 'NONE',  ( 0.2903256038615220636, 4.748660027621867563, 0.1207610085887053653 ) ) ;
#171 = CARTESIAN_POINT ( 'NONE',  ( 0.2923287055106771337, -0.01339285724039953988, 0.2123892367102621359 ) ) ;
#172 = CARTESIAN_POINT ( 'NONE',  ( 0.3119530872320841475, 3.973196682663843848, 0.04116800644467977222 ) ) ;
#173 = ORIENTED_EDGE ( 'NONE', *, *, #22442, .F. ) ;
#174 = CARTESIAN_POINT ( 'NONE',  ( 2.326421213736078119E-17, 0.02946428561674332633, -0.3799334167787516980 ) ) ;
#175 = VERTEX_POINT ( 'NONE', #18914 ) ;
#176 = CYLINDRICAL_SURFACE ( 'NONE', #2581, 0.01874999999999997155 ) ;
#177 = CARTESIAN_POINT ( 'NONE',  ( -0.3070879998666070088, 4.670587574863169777, 0.05874933755621322695 ) ) ;
#178 = CC_DESIGN_PERSON_AND_ORGANIZATION_ASSIGNMENT ( #23063, #2955, ( #8009 ) ) ;
#179 = EDGE_CURVE ( 'NONE', #769, #10349, #4149, .T. ) ;
#180 = CARTESIAN_POINT ( 'NONE',  ( 5.178964085587577574E-17, 4.144527777853642903, 0.2819296736111110979 ) ) ;
#181 = CARTESIAN_POINT ( 'NONE',  ( -0.2720287551442893137, -0.3842100023554003152, 0.4182004018663288414 ) ) ;
#182 = CARTESIAN_POINT ( 'NONE',  ( 0.2723623684625768870, -0.3840173906162817064, 0.09139303015897912164 ) ) ;
#183 = CARTESIAN_POINT ( 'NONE',  ( -0.2206173157302027676, 3.891055555555554601, 0.2206173157302028787 ) ) ;
#184 = CARTESIAN_POINT ( 'NONE',  ( 0.1292346314604058410, 4.686194444596177178, 0.3119999999999998885 ) ) ;
#185 = CARTESIAN_POINT ( 'NONE',  ( 0.07199389927938498746, 4.795915137278597307, 0.3053389904577915592 ) ) ;
#186 = CARTESIAN_POINT ( 'NONE',  ( 0.1993543840281267465, 4.373694444520309865, 0.1993543840281266633 ) ) ;
#187 = CARTESIAN_POINT ( 'NONE',  ( -0.4749999999999999778, 3.575000000000000622, -0.09499999999999995948 ) ) ;
#188 = ORIENTED_EDGE ( 'NONE', *, *, #16033, .F. ) ;
#189 = CARTESIAN_POINT ( 'NONE',  ( -6.979263641208234666E-17, 0.1901785713310290005, 0.3799334167787516980 ) ) ;
#190 = VECTOR ( 'NONE', #20560, 39.37007874015748143 ) ;
#191 = CARTESIAN_POINT ( 'NONE',  ( -0.03922876767354999128, 0.06005265186466097332, 0.3076901691082670753 ) ) ;
#192 = ORIENTED_EDGE ( 'NONE', *, *, #14503, .T. ) ;
#193 = APPROVAL_STATUS ( 'not_yet_approved' ) ;
#194 = ORGANIZATION ( 'NAUO-ORG6', 'UNSPECIFIED', 'UNSPECIFIED' ) ;
#195 = CARTESIAN_POINT ( 'NONE',  ( 0.4570242136016807732, 0.2774028246161672207, 0.04874733047933993424 ) ) ;
#196 = CARTESIAN_POINT ( 'NONE',  ( -1.726321361862525858E-17, 5.172305555631420582, -0.2819296736111110979 ) ) ;
#197 = APPROVAL_PERSON_ORGANIZATION ( #4573, #17441, #23090 ) ;
#198 = CARTESIAN_POINT ( 'NONE',  ( -0.2819296736111110424, 3.925777777853644235, 0.1167790944451424923 ) ) ;
#199 = EDGE_CURVE ( 'NONE', #21090, #21943, #17206, .T. ) ;
#200 = CARTESIAN_POINT ( 'NONE',  ( -6.389700406101856968E-07, 4.404919069638722817, 0.3119999999986028949 ) ) ;
#201 = CARTESIAN_POINT ( 'NONE',  ( -0.1116596296178199582, 0.3723214284738861068, -0.3436530038418508792 ) ) ;
#202 = ORIENTED_EDGE ( 'NONE', *, *, #20793, .T. ) ;
#203 = CARTESIAN_POINT ( 'NONE',  ( -0.2764156081756484196, -0.1144950937579609362, 0.2584722222222254340 ) ) ;
#204 = CARTESIAN_POINT ( 'NONE',  ( 0.1167790944451423535, 0.5944444443685777957, 0.2819296736111110979 ) ) ;
#205 = CARTESIAN_POINT ( 'NONE',  ( 0.1954553509668047195, 0.1954553509668046085, -0.09916666666666627827 ) ) ;
#206 = CARTESIAN_POINT ( 'NONE',  ( 0.2819296736111110424, 4.898000000075866112, -0.1167790944451423396 ) ) ;
#207 = FACE_OUTER_BOUND ( 'NONE', #7341, .T. ) ;
#208 = VECTOR ( 'NONE', #13056, 39.37007874015748854 ) ;
#209 = EDGE_CURVE ( 'NONE', #14671, #23965, #20865, .T. ) ;
#210 = CARTESIAN_POINT ( 'NONE',  ( 0.1167790944451422702, 4.946611111186975940, -0.2819296736111110424 ) ) ;
#211 = CARTESIAN_POINT ( 'NONE',  ( -0.4587679311106390156, 0.1778692279407495247, 0.4165783083332769698 ) ) ;
#212 = CARTESIAN_POINT ( 'NONE',  ( 0.2409776823595090323, 4.857164591472093562, 0.1984146367410583867 ) ) ;
#213 = DIRECTION ( 'NONE',  ( 0.000000000000000000, 0.000000000000000000, -1.000000000000000000 ) ) ;
#214 = CARTESIAN_POINT ( 'NONE',  ( 0.000000000000000000, 0.000000000000000000, 0.000000000000000000 ) ) ;
#215 = CARTESIAN_POINT ( 'NONE',  ( 5.731347020009612645E-17, 4.453555555555555046, 0.3119999999999999996 ) ) ;
#216 = CARTESIAN_POINT ( 'NONE',  ( -0.4000000000000000222, 0.2964285714285713191, 0.1299678784931624920 ) ) ;
#217 = CARTESIAN_POINT ( 'NONE',  ( 0.1292346314604056745, 0.3548611109593781676, -0.3119999999999999996 ) ) ;
#218 = CARTESIAN_POINT ( 'NONE',  ( 0.0007558196063935046592, 4.988256100791213399, -0.3119993132609195641 ) ) ;
#219 = CARTESIAN_POINT ( 'NONE',  ( -0.1042511535495848213, 3.735277012539861108, 0.2940678913504243819 ) ) ;
#220 = CC_DESIGN_APPROVAL ( #3735, ( #11526 ) ) ;
#221 = CARTESIAN_POINT ( 'NONE',  ( 0.3010133589939812948, 4.583146549113322976, 0.08341395606948878716 ) ) ;
#222 = EDGE_LOOP ( 'NONE', ( #15258, #20652 ) ) ;
#223 = CARTESIAN_POINT ( 'NONE',  ( -0.4226370775080299236, -0.2972562468964969895, 0.3901966308178843601 ) ) ;
#224 = AXIS2_PLACEMENT_3D ( 'NONE', #22932, #10391, #12107 ) ;
#225 = CARTESIAN_POINT ( 'NONE',  ( 0.1785406736446525644, 4.649568862857817564, -0.2599013730876763573 ) ) ;
#226 = EDGE_CURVE ( 'NONE', #20003, #8247, #7693, .T. ) ;
#227 = CARTESIAN_POINT ( 'NONE',  ( -0.2230971623002953874, 0.2230971623002954152, -0.1634027777777777302 ) ) ;
#228 = EDGE_CURVE ( 'NONE', #4857, #5916, #14256, .T. ) ;
#229 = PLANE ( 'NONE',  #11115 ) ;
#230 = DIRECTION ( 'NONE',  ( -0.000000000000000000, 0.2588190451025213501, -0.9659258262890680902 ) ) ;
#231 = ORIENTED_EDGE ( 'NONE', *, *, #20196, .T. ) ;
#232 = CC_DESIGN_SECURITY_CLASSIFICATION ( #16981, ( #9980 ) ) ;
#233 = CARTESIAN_POINT ( 'NONE',  ( -0.3613381517857143232, 0.1901785713310290005, -4.425116109941954795E-17 ) ) ;
#234 = CARTESIAN_POINT ( 'NONE',  ( 0.1993543840281266355, 0.4173611110352444808, 0.1993543840281267465 ) ) ;
#235 = CARTESIAN_POINT ( 'NONE',  ( 0.4450000000000002842, 0.05000000000000028727, -2.591000000000000192 ) ) ;
#236 = CARTESIAN_POINT ( 'NONE',  ( 0.01030609754475048101, 0.1800000000000000211, -1.243000000000000105 ) ) ;
#237 = CARTESIAN_POINT ( 'NONE',  ( -0.3120000000000000551, 0.1604166666666663188, 0.1292346314604056190 ) ) ;
#238 = CARTESIAN_POINT ( 'NONE',  ( 0.000000000000000000, 0.2764156081756484196, 0.08138888888889070361 ) ) ;
#239 = EDGE_CURVE ( 'NONE', #8265, #17235, #2483, .T. ) ;
#240 = CARTESIAN_POINT ( 'NONE',  ( -0.3003085958321041748, 5.103171429360789269, -0.08162789287472543842 ) ) ;
#241 = CARTESIAN_POINT ( 'NONE',  ( 0.4687500000000002776, 0.02218466657066830647, 0.4181373467287273216 ) ) ;
#242 = CARTESIAN_POINT ( 'NONE',  ( 0.1292346314604056745, 0.2506944444444441089, -0.3119999999999999996 ) ) ;
#243 = CARTESIAN_POINT ( 'NONE',  ( -1.910449006669871087E-17, 5.092444444444443441, -0.3119999999999999996 ) ) ;
#244 = CLOSED_SHELL ( 'NONE', ( #18887, #14949, #5630, #5410, #4548, #13026, #18679, #3074, #17557, #11622, #8845, #6138, #15005, #14422, #9769, #4119, #5737 ) ) ;
#245 = CARTESIAN_POINT ( 'NONE',  ( 0.2819296736111110979, 4.279944444520310753, 0.1167790944451422425 ) ) ;
#246 = CARTESIAN_POINT ( 'NONE',  ( -0.3119999999999999996, 3.825083333333333169, -0.1292346314604056468 ) ) ;
#247 = CARTESIAN_POINT ( 'NONE',  ( -9.626299801968715084E-16, 0.4089285712334866374, -0.4000000000000000222 ) ) ;
#248 = ORIENTED_EDGE ( 'NONE', *, *, #15243, .F. ) ;
#249 = CARTESIAN_POINT ( 'NONE',  ( -0.4648120342697260043, -0.2865046371989117269, 0.04342012612512782810 ) ) ;
#250 = CARTESIAN_POINT ( 'NONE',  ( 0.1167790944451424368, 4.981333333409198261, 0.2819296736111110424 ) ) ;
#251 = APPROVAL_PERSON_ORGANIZATION ( #2689, #19998, #9894 ) ;
#252 = LINE ( 'NONE', #17321, #13881 ) ;
#253 = CARTESIAN_POINT ( 'NONE',  ( -5.731347020009612645E-17, 0.6083333331816004330, 0.3119999999999999996 ) ) ;
#254 = CARTESIAN_POINT ( 'NONE',  ( 0.2819296736111111534, 4.599388888964754507, 0.1167790944451422563 ) ) ;
#255 = COORDINATED_UNIVERSAL_TIME_OFFSET ( 0, 0, .AHEAD. ) ;
#256 = CARTESIAN_POINT ( 'NONE',  ( 0.1292346314604058410, 4.290361111111110404, 0.3119999999999998885 ) ) ;
#257 = CARTESIAN_POINT ( 'NONE',  ( 0.000000000000000000, 0.2764156081756484196, 0.02583333333333468970 ) ) ;
#258 = CARTESIAN_POINT ( 'NONE',  ( 0.1993543840281266910, 0.5006944443685779067, -0.1993543840281266910 ) ) ;
#259 = ORIENTED_EDGE ( 'NONE', *, *, #15539, .F. ) ;
#260 = CARTESIAN_POINT ( 'NONE',  ( -0.2819296736111110424, 0.1291666665908000611, -0.1167790944451423396 ) ) ;
#261 = DIRECTION ( 'NONE',  ( -0.5773502691896257311, -0.5773502691896257311, 0.5773502691896257311 ) ) ;
#262 = CARTESIAN_POINT ( 'NONE',  ( -0.3949525857693607089, 5.436648244187127775E-19, 0.06334394204733222178 ) ) ;
#263 = CARTESIAN_POINT ( 'NONE',  ( -7.726019084026502927E-17, 0.1678571428571428159, 0.4205848896953069405 ) ) ;
#264 = CARTESIAN_POINT ( 'NONE',  ( -0.2230971623002953874, 0.2230971623002954152, 0.05534722222222363680 ) ) ;
#265 = ADVANCED_FACE ( 'NONE', ( #22443 ), #4898, .F. ) ;
#266 = CARTESIAN_POINT ( 'NONE',  ( -0.3125000000000000000, 1.913510623667739771E-17, 0.01194444444444589179 ) ) ;
#267 = FACE_OUTER_BOUND ( 'NONE', #5733, .T. ) ;
#268 = CARTESIAN_POINT ( 'NONE',  ( 0.1167790944451423535, 0.1916666665908000056, 0.2819296736111110979 ) ) ;
#269 = CARTESIAN_POINT ( 'NONE',  ( 0.2819296736111110979, 0.1465277777019111383, 0.000000000000000000 ) ) ;
#270 = CARTESIAN_POINT ( 'NONE',  ( -0.1167790944451423535, 4.321611111186976828, 0.2819296736111110424 ) ) ;
#271 = CARTESIAN_POINT ( 'NONE',  ( -0.3236067977499790249, 0.1482142855192009057, 0.2351141009169892271 ) ) ;
#272 = CARTESIAN_POINT ( 'NONE',  ( -1.726321361862525858E-17, 4.852861111186976828, -0.2819296736111110979 ) ) ;
#273 = CARTESIAN_POINT ( 'NONE',  ( 0.2819296736111111534, 4.377166666742532186, 0.1167790944451422563 ) ) ;
#274 = CARTESIAN_POINT ( 'NONE',  ( -6.528214817076446933E-07, 5.071585437816050757, 0.3119999999985565986 ) ) ;
#275 = AXIS2_PLACEMENT_3D ( 'NONE', #1586, #7436, #11218 ) ;
#276 = DIRECTION ( 'NONE',  ( 0.000000000000000000, 0.000000000000000000, -1.000000000000000000 ) ) ;
#277 = CARTESIAN_POINT ( 'NONE',  ( 0.2206173157302027954, 4.092444444596176290, -0.2206173157302028232 ) ) ;
#278 = DIRECTION ( 'NONE',  ( 0.000000000000000000, 1.000000000000000000, 0.000000000000000000 ) ) ;
#279 = PLANE ( 'NONE',  #11488 ) ;
#280 = VERTEX_POINT ( 'NONE', #11359 ) ;
#281 = DATE_AND_TIME ( #645, #12298 ) ;
#282 = CARTESIAN_POINT ( 'NONE',  ( 0.06335377612981443751, 0.4464733670030167634, 0.4000000000000000222 ) ) ;
#283 = CARTESIAN_POINT ( 'NONE',  ( 0.3003475124358242487, 3.066692553488282957, 3.638968604327563749 ) ) ;
#284 = CARTESIAN_POINT ( 'NONE',  ( -0.1566814371109810367, 4.992845198620254443, -0.2728731690866343929 ) ) ;
#285 = ORIENTED_EDGE ( 'NONE', *, *, #22981, .F. ) ;
#286 = CARTESIAN_POINT ( 'NONE',  ( 0.2206173157302028232, 0.5180555554038226429, -0.2206173157302028232 ) ) ;
#287 = VECTOR ( 'NONE', #16443, 39.37007874015748854 ) ;
#288 = ORIENTED_EDGE ( 'NONE', *, *, #4311, .T. ) ;
#289 = DIRECTION ( 'NONE',  ( -0.8660254037844382635, 0.000000000000000000, -0.5000000000000004441 ) ) ;
#290 = CARTESIAN_POINT ( 'NONE',  ( 0.07990078027837828334, 0.4951351403631162329, 0.4110703004652723758 ) ) ;
#291 = CARTESIAN_POINT ( 'NONE',  ( -0.3120000000000000551, 0.5493055555555551583, 0.1292346314604056190 ) ) ;
#292 = CARTESIAN_POINT ( 'NONE',  ( -0.3613381517857144343, -0.03839285724039952913, 0.1174058825155740171 ) ) ;
#293 = LINE ( 'NONE', #9080, #3063 ) ;
#294 = EDGE_CURVE ( 'NONE', #17172, #5916, #19316, .T. ) ;
#295 =( BOUNDED_SURFACE ( )  B_SPLINE_SURFACE ( 1, 2, ( 
 ( #11604, #5858, #4030, #20737, #17207, #9647, #17082, #11849, #19034, #19147, #372, #19266, #15255, #22685, #2335, #22805, #3045, #10254, #21459, #13912, #4742, #14142, #14385, #6459, #2799, #21571, #8525, #6578, #2687, #6946, #19389, #23628, #23268, #21341, #17922, #2920, #14028, #19505, #4865, #12331, #1334, #21813, #4628, #17801, #19746, #14263, #10379, #12448, #6822, #8764, #12214, #10492, #12095, #1093, #10139, #19622, #17563, #16093, #15968, #1217, #11976, #23389, #6696, #21698, #17681, #15850, #23149, #19864, #971, #854, #8645, #8283, #23507, #4983, #10609, #3159, #18038, #16216, #8400, #15736, #7188, #21927, #12568, #14631, #16456, #3524, #10973, #23997, #14758, #10852, #16576, #18518, #22053, #12939, #11088, #24115, #16694, #23746, #14993, #16819, #13054, #1808, #5102, #18160, #102, #5590, #19988, #20350, #9253, #5220, #5348, #7430, #14877, #12816, #18400, #22294, #7307, #3401, #20233, #20473, #3769, #3641, #11210, #18639, #1930, #3275, #9377, #10729, #23868, #7543, #1457, #1694, #8892, #16333, #7070, #14508, #9130, #22175, #18280, #12693, #5474, #1576, #20110, #9013, #22660, #16930, #2540, #9497, #2424, #5829, #15114, #9865, #706, #17178, #22415, #15347, #9742, #21068, #13406, #17050, #19119, #17293, #22540, #4122, #19236, #5718, #13652, #11695, #3885, #2057, #464, #11579, #20949, #7896, #4360, #4243, #17413, #9989, #15230 ),
 ( #11816, #19007, #227, #11453, #22774, #6069, #2187, #13536, #9618, #8134, #2304, #20830, #344, #585, #13177, #20590, #18760, #11330, #22894, #8016, #15468, #18885, #6188, #7784, #7663, #5949, #13294, #20709, #4003, #4954, #19834, #13884, #19476, #12300, #2770, #21312, #23238, #10344, #14113, #10223, #12419, #8491, #2884, #14231, #6546, #17649, #19714, #3017, #15705, #21427, #3132, #15585, #6792, #4832, #21190, #19360, #17771, #4715, #21544, #1063, #21668, #10464, #10584, #18012, #8367, #938, #15819, #4479, #11945, #17893, #1307, #12186, #2658, #4603, #15934, #23358, #13997, #6668, #19592, #23009, #1186, #8621, #16062, #23477, #6311, #13764, #10110, #17533, #825, #8253, #23120, #12063, #6429, #18250, #14353, #16429, #12787, #9099, #22146, #22266, #13029, #7040, #12662, #5444, #20080, #14479, #23838, #3491, #7281, #3373, #5563, #3249, #18614, #20443, #16666, #12908, #8732, #21785, #3740, #9229, #16187, #16547, #20322, #8858, #1547, #14730, #3609, #8984, #14601, #11062, #20205, #21903, #7160, #24089, #18491, #1784, #23969, #7401, #14851, #6914, #11186, #23599, #10824, #5071, #12541, #22024, #19961, #10697, #18133, #1431, #5322, #1666, #5193, #16302, #10943, #18371, #23715, #15086, #2155, #20563, #6157, #13150, #6039, #9468, #18734, #13506, #4331, #20802, #1905, #3974, #9711, #7869, #20920, #4213, #2031, #22635, #17022, #13379, #2275 ) ),
 .UNSPECIFIED., .F., .F., .F. ) 
 B_SPLINE_SURFACE_WITH_KNOTS ( ( 2, 2 ),
 ( 3, 2, 2, 2, 2, 2, 2, 2, 2, 2, 2, 2, 2, 2, 2, 2, 2, 2, 2, 2, 2, 2, 2, 2, 2, 2, 2, 2, 2, 2, 2, 2, 2, 2, 2, 2, 2, 2, 2, 2, 2, 2, 2, 2, 2, 2, 2, 2, 2, 2, 2, 2, 2, 2, 2, 2, 2, 2, 2, 2, 2, 2, 2, 2, 2, 2, 2, 2, 2, 2, 2, 2, 2, 2, 2, 2, 2, 2, 2, 2, 2, 2, 2, 2, 2, 2, 2, 2, 2, 3 ),
 ( 0.000000000000000000, 1.000000000000000000 ),
 ( 0.000000000000000000, 0.01041666666666666609, 0.02083333333333333218, 0.03125000000000000000, 0.04166666666666666435, 0.05208333333333333565, 0.06250000000000000000, 0.07291666666666667129, 0.08333333333333332871, 0.09375000000000000000, 0.1041666666666666713, 0.1145833333333333287, 0.1250000000000000000, 0.1354166666666666574, 0.1458333333333333426, 0.1562500000000000000, 0.1666666666666666574, 0.1770833333333333426, 0.1875000000000000000, 0.1979166666666666574, 0.2083333333333333426, 0.2187500000000000000, 0.2291666666666666574, 0.2395833333333333426, 0.2500000000000000000, 0.2604166666666666852, 0.2708333333333333148, 0.2812500000000000000, 0.2916666666666666852, 0.3020833333333333148, 0.3125000000000000000, 0.3229166666666666852, 0.3333333333333333148, 0.3437500000000000000, 0.3541666666666666852, 0.3645833333333333148, 0.3750000000000000000, 0.3854166666666666852, 0.3958333333333333148, 0.4062500000000000000, 0.4166666666666666852, 0.4270833333333333148, 0.4375000000000000000, 0.4479166666666666852, 0.4583333333333333148, 0.4687500000000000000, 0.4791666666666666852, 0.4895833333333333148, 0.5000000000000000000, 0.5104166666666666297, 0.5208333333333333703, 0.5312500000000000000, 0.5416666666666666297, 0.5520833333333333703, 0.5625000000000000000, 0.5729166666666666297, 0.5833333333333333703, 0.5937500000000000000, 0.6041666666666666297, 0.6145833333333333703, 0.6250000000000000000, 0.6354166666666666297, 0.6458333333333333703, 0.6562500000000000000, 0.6666666666666666297, 0.6770833333333333703, 0.6875000000000000000, 0.6979166666666666297, 0.7083333333333333703, 0.7187500000000000000, 0.7291666666666666297, 0.7395833333333333703, 0.7500000000000000000, 0.7604166666666666297, 0.7708333333333333703, 0.7812500000000000000, 0.7916666666666666297, 0.8020833333333333703, 0.8125000000000000000, 0.8229166666666666297, 0.8333333333333333703, 0.8437500000000000000, 0.8541666666666666297, 0.8645833333333333703, 0.8750000000000000000, 0.8854166666666666297, 0.8958333333333333703, 0.9062500000000000000, 0.9166666666666666297, 0.9270833333333333703 ),
 .UNSPECIFIED. ) 
 GEOMETRIC_REPRESENTATION_ITEM ( )  RATIONAL_B_SPLINE_SURFACE ( (
 ( 1.000000000000000000, 0.9238795325112867385, 1.000000000000000000, 0.9238795325112867385, 1.000000000000000000, 0.9238795325112867385, 1.000000000000000000, 0.9238795325112867385, 1.000000000000000000, 0.9238795325112867385, 1.000000000000000000, 0.9238795325112867385, 1.000000000000000000, 0.9238795325112867385, 1.000000000000000000, 0.9238795325112867385, 1.000000000000000000, 0.9238795325112867385, 1.000000000000000000, 0.9238795325112867385, 1.000000000000000000, 0.9238795325112867385, 1.000000000000000000, 0.9238795325112867385, 1.000000000000000000, 0.9238795325112867385, 1.000000000000000000, 0.9238795325112867385, 1.000000000000000000, 0.9238795325112867385, 1.000000000000000000, 0.9238795325112867385, 1.000000000000000000, 0.9238795325112867385, 1.000000000000000000, 0.9238795325112867385, 1.000000000000000000, 0.9238795325112867385, 1.000000000000000000, 0.9238795325112867385, 1.000000000000000000, 0.9238795325112867385, 1.000000000000000000, 0.9238795325112867385, 1.000000000000000000, 0.9238795325112867385, 1.000000000000000000, 0.9238795325112867385, 1.000000000000000000, 0.9238795325112867385, 1.000000000000000000, 0.9238795325112867385, 1.000000000000000000, 0.9238795325112867385, 1.000000000000000000, 0.9238795325112867385, 1.000000000000000000, 0.9238795325112867385, 1.000000000000000000, 0.9238795325112867385, 1.000000000000000000, 0.9238795325112867385, 1.000000000000000000, 0.9238795325112867385, 1.000000000000000000, 0.9238795325112867385, 1.000000000000000000, 0.9238795325112867385, 1.000000000000000000, 0.9238795325112867385, 1.000000000000000000, 0.9238795325112867385, 1.000000000000000000, 0.9238795325112867385, 1.000000000000000000, 0.9238795325112867385, 1.000000000000000000, 0.9238795325112867385, 1.000000000000000000, 0.9238795325112867385, 1.000000000000000000, 0.9238795325112867385, 1.000000000000000000, 0.9238795325112867385, 1.000000000000000000, 0.9238795325112867385, 1.000000000000000000, 0.9238795325112867385, 1.000000000000000000, 0.9238795325112867385, 1.000000000000000000, 0.9238795325112867385, 1.000000000000000000, 0.9238795325112867385, 1.000000000000000000, 0.9238795325112867385, 1.000000000000000000, 0.9238795325112867385, 1.000000000000000000, 0.9238795325112867385, 1.000000000000000000, 0.9238795325112867385, 1.000000000000000000, 0.9238795325112867385, 1.000000000000000000, 0.9238795325112867385, 1.000000000000000000, 0.9238795325112867385, 1.000000000000000000, 0.9238795325112867385, 1.000000000000000000, 0.9238795325112867385, 1.000000000000000000, 0.9238795325112867385, 1.000000000000000000, 0.9238795325112867385, 1.000000000000000000, 0.9238795325112867385, 1.000000000000000000, 0.9238795325112867385, 1.000000000000000000, 0.9238795325112867385, 1.000000000000000000, 0.9238795325112867385, 1.000000000000000000, 0.9238795325112867385, 1.000000000000000000, 0.9238795325112867385, 1.000000000000000000, 0.9238795325112867385, 1.000000000000000000, 0.9238795325112867385, 1.000000000000000000, 0.9238795325112867385, 1.000000000000000000, 0.9238795325112867385, 1.000000000000000000, 0.9238795325112867385, 1.000000000000000000, 0.9238795325112867385, 1.000000000000000000, 0.9238795325112867385, 1.000000000000000000, 0.9238795325112867385, 1.000000000000000000, 0.9238795325112867385, 1.000000000000000000, 0.9238795325112867385, 1.000000000000000000, 0.9238795325112867385, 1.000000000000000000, 0.9238795325112867385, 1.000000000000000000, 0.9238795325112867385, 1.000000000000000000, 0.9238795325112867385, 1.000000000000000000, 0.9238795325112867385, 1.000000000000000000, 0.9238795325112867385, 1.000000000000000000, 0.9238795325112867385, 1.000000000000000000, 0.9238795325112867385, 1.000000000000000000, 0.9238795325112867385, 1.000000000000000000, 0.9238795325112867385, 1.000000000000000000, 0.9238795325112867385, 1.000000000000000000, 0.9238795325112867385, 1.000000000000000000, 0.9238795325112867385, 1.000000000000000000, 0.9238795325112867385, 1.000000000000000000, 0.9238795325112867385, 1.000000000000000000),
 ( 1.000000000000000000, 0.9238795325112867385, 1.000000000000000000, 0.9238795325112867385, 1.000000000000000000, 0.9238795325112867385, 1.000000000000000000, 0.9238795325112867385, 1.000000000000000000, 0.9238795325112867385, 1.000000000000000000, 0.9238795325112867385, 1.000000000000000000, 0.9238795325112867385, 1.000000000000000000, 0.9238795325112867385, 1.000000000000000000, 0.9238795325112867385, 1.000000000000000000, 0.9238795325112867385, 1.000000000000000000, 0.9238795325112867385, 1.000000000000000000, 0.9238795325112867385, 1.000000000000000000, 0.9238795325112867385, 1.000000000000000000, 0.9238795325112867385, 1.000000000000000000, 0.9238795325112867385, 1.000000000000000000, 0.9238795325112867385, 1.000000000000000000, 0.9238795325112867385, 1.000000000000000000, 0.9238795325112867385, 1.000000000000000000, 0.9238795325112867385, 1.000000000000000000, 0.9238795325112867385, 1.000000000000000000, 0.9238795325112867385, 1.000000000000000000, 0.9238795325112867385, 1.000000000000000000, 0.9238795325112867385, 1.000000000000000000, 0.9238795325112867385, 1.000000000000000000, 0.9238795325112867385, 1.000000000000000000, 0.9238795325112867385, 1.000000000000000000, 0.9238795325112867385, 1.000000000000000000, 0.9238795325112867385, 1.000000000000000000, 0.9238795325112867385, 1.000000000000000000, 0.9238795325112867385, 1.000000000000000000, 0.9238795325112867385, 1.000000000000000000, 0.9238795325112867385, 1.000000000000000000, 0.9238795325112867385, 1.000000000000000000, 0.9238795325112867385, 1.000000000000000000, 0.9238795325112867385, 1.000000000000000000, 0.9238795325112867385, 1.000000000000000000, 0.9238795325112867385, 1.000000000000000000, 0.9238795325112867385, 1.000000000000000000, 0.9238795325112867385, 1.000000000000000000, 0.9238795325112867385, 1.000000000000000000, 0.9238795325112867385, 1.000000000000000000, 0.9238795325112867385, 1.000000000000000000, 0.9238795325112867385, 1.000000000000000000, 0.9238795325112867385, 1.000000000000000000, 0.9238795325112867385, 1.000000000000000000, 0.9238795325112867385, 1.000000000000000000, 0.9238795325112867385, 1.000000000000000000, 0.9238795325112867385, 1.000000000000000000, 0.9238795325112867385, 1.000000000000000000, 0.9238795325112867385, 1.000000000000000000, 0.9238795325112867385, 1.000000000000000000, 0.9238795325112867385, 1.000000000000000000, 0.9238795325112867385, 1.000000000000000000, 0.9238795325112867385, 1.000000000000000000, 0.9238795325112867385, 1.000000000000000000, 0.9238795325112867385, 1.000000000000000000, 0.9238795325112867385, 1.000000000000000000, 0.9238795325112867385, 1.000000000000000000, 0.9238795325112867385, 1.000000000000000000, 0.9238795325112867385, 1.000000000000000000, 0.9238795325112867385, 1.000000000000000000, 0.9238795325112867385, 1.000000000000000000, 0.9238795325112867385, 1.000000000000000000, 0.9238795325112867385, 1.000000000000000000, 0.9238795325112867385, 1.000000000000000000, 0.9238795325112867385, 1.000000000000000000, 0.9238795325112867385, 1.000000000000000000, 0.9238795325112867385, 1.000000000000000000, 0.9238795325112867385, 1.000000000000000000, 0.9238795325112867385, 1.000000000000000000, 0.9238795325112867385, 1.000000000000000000, 0.9238795325112867385, 1.000000000000000000, 0.9238795325112867385, 1.000000000000000000, 0.9238795325112867385, 1.000000000000000000, 0.9238795325112867385, 1.000000000000000000, 0.9238795325112867385, 1.000000000000000000, 0.9238795325112867385, 1.000000000000000000, 0.9238795325112867385, 1.000000000000000000, 0.9238795325112867385, 1.000000000000000000, 0.9238795325112867385, 1.000000000000000000, 0.9238795325112867385, 1.000000000000000000, 0.9238795325112867385, 1.000000000000000000, 0.9238795325112867385, 1.000000000000000000, 0.9238795325112867385, 1.000000000000000000, 0.9238795325112867385, 1.000000000000000000, 0.9238795325112867385, 1.000000000000000000, 0.9238795325112867385, 1.000000000000000000, 0.9238795325112867385, 1.000000000000000000, 0.9238795325112867385, 1.000000000000000000) ) ) 
 REPRESENTATION_ITEM ( '' )  SURFACE ( )  );
#296 = EDGE_LOOP ( 'NONE', ( #12056, #1155, #20586, #17433 ) ) ;
#297 = CARTESIAN_POINT ( 'NONE',  ( 0.2923287055106771337, 0.1616071427596004473, -0.2123892367102620249 ) ) ;
#298 = PLANE ( 'NONE',  #11943 ) ;
#299 = CARTESIAN_POINT ( 'NONE',  ( 5.731347020009612645E-17, 4.064666666666665762, 0.3119999999999999996 ) ) ;
#300 = CARTESIAN_POINT ( 'NONE',  ( 0.1167790944451422702, 4.057722222298087544, -0.2819296736111110424 ) ) ;
#301 = CARTESIAN_POINT ( 'NONE',  ( -0.3874422277197493436, -0.3175760028958487524, 0.4114235598616964862 ) ) ;
#302 = DIRECTION ( 'NONE',  ( 1.000000000000000000, -0.000000000000000000, 1.224646799147353207E-16 ) ) ;
#303 = CARTESIAN_POINT ( 'NONE',  ( -0.2206173157302028232, 3.932722222222221120, -0.2206173157302028232 ) ) ;
#304 = CARTESIAN_POINT ( 'NONE',  ( 0.1292346314604056190, 4.762583333485065573, -0.3119999999999999996 ) ) ;
#305 = CARTESIAN_POINT ( 'NONE',  ( -0.2819296736111110979, 4.863277777853643791, -0.1167790944451422980 ) ) ;
#306 = ORIENTED_EDGE ( 'NONE', *, *, #17817, .T. ) ;
#307 = ADVANCED_FACE ( 'NONE', ( #10137 ), #17850, .F. ) ;
#308 = CARTESIAN_POINT ( 'NONE',  ( 0.1167790944451422702, 4.335500000075866112, -0.2819296736111110424 ) ) ;
#309 = AXIS2_PLACEMENT_3D ( 'NONE', #6087, #20725, #7680 ) ;
#310 = CARTESIAN_POINT ( 'NONE',  ( 0.000000000000000000, 0.000000000000000000, 0.2041999999999999926 ) ) ;
#311 = ORIENTED_EDGE ( 'NONE', *, *, #12442, .F. ) ;
#312 = CARTESIAN_POINT ( 'NONE',  ( -0.2233192592356399442, 0.09017857133102903655, -0.3073725909049499494 ) ) ;
#313 = ORIENTED_EDGE ( 'NONE', *, *, #4837, .T. ) ;
#314 = VERTEX_POINT ( 'NONE', #21339 ) ;
#315 = DATE_AND_TIME ( #16900, #598 ) ;
#316 = SPHERICAL_SURFACE ( 'NONE', #20439, 0.3119999999999999996 ) ;
#317 = CARTESIAN_POINT ( 'NONE',  ( -0.1167790944451423257, 5.120222222298088433, -0.2819296736111110424 ) ) ;
#318 = CARTESIAN_POINT ( 'NONE',  ( -0.2819296736111110424, 3.814666666742532630, 0.1167790944451424923 ) ) ;
#319 = CARTESIAN_POINT ( 'NONE',  ( 0.04075291810813885807, 4.431559223094041045, -0.3099974353593557552 ) ) ;
#320 = CARTESIAN_POINT ( 'NONE',  ( 0.1954553509668046640, -0.1954553509668047195, 0.3383333333333371495 ) ) ;
#321 = DIRECTION ( 'NONE',  ( -0.8660254037844443697, 0.000000000000000000, -0.4999999999999902300 ) ) ;
#322 = CIRCLE ( 'NONE', #10458, 1.200750000000023299 ) ;
#323 = CARTESIAN_POINT ( 'NONE',  ( 0.2764156081756483641, 0.1144950937579610195, 0.3418055555555594149 ) ) ;
#324 = CARTESIAN_POINT ( 'NONE',  ( 0.2819296736111110979, 0.6083333332574668573, -0.1167790944451422980 ) ) ;
#325 = CARTESIAN_POINT ( 'NONE',  ( 0.1954553509668046640, -0.1954553509668047195, -0.05749999999999928085 ) ) ;
#326 = CARTESIAN_POINT ( 'NONE',  ( -0.2819296736111110979, 4.977861111186976828, 0.000000000000000000 ) ) ;
#327 = CARTESIAN_POINT ( 'NONE',  ( -1.910449006669871087E-17, 3.925777777777776922, -0.3119999999999999996 ) ) ;
#328 = CARTESIAN_POINT ( 'NONE',  ( 0.2819296736111110979, 4.654944444520309865, 0.1167790944451422425 ) ) ;
#329 = CARTESIAN_POINT ( 'NONE',  ( 0.4000000000000000222, 0.4312499999024575481, 0.000000000000000000 ) ) ;
#330 = CARTESIAN_POINT ( 'NONE',  ( 0.08682016143536398778, 4.851954871454551288, 0.3004229350962410172 ) ) ;
#331 = CARTESIAN_POINT ( 'NONE',  ( -0.3341642768485558745, -2.437189573335733509E-18, 0.2058836888633447382 ) ) ;
#332 = CARTESIAN_POINT ( 'NONE',  ( 2.284599161994749217, 2.687712728237018567, -2.476240473580834323 ) ) ;
#333 = CARTESIAN_POINT ( 'NONE',  ( -0.3119999999999998885, 4.609805555555555046, 0.1292346314604058410 ) ) ;
#334 = CARTESIAN_POINT ( 'NONE',  ( -0.1167790944451423535, 3.807722222298087988, 0.2819296736111110979 ) ) ;
#335 = CARTESIAN_POINT ( 'NONE',  ( -1.910449006669871087E-17, 4.203555555555555046, -0.3119999999999999996 ) ) ;
#336 = CARTESIAN_POINT ( 'NONE',  ( -0.2472135954999579999, 0.2321428571428570953, 0.3402603233408160732 ) ) ;
#337 = ORIENTED_EDGE ( 'NONE', *, *, #3360, .F. ) ;
#338 = CARTESIAN_POINT ( 'NONE',  ( 0.03916719867818912321, 4.598255416773466386, -0.3119999648250499358 ) ) ;
#339 = EDGE_LOOP ( 'NONE', ( #18728, #8488, #19395, #1831 ) ) ;
#340 = CARTESIAN_POINT ( 'NONE',  ( -0.4620259694561524855, 0.2880908832651556950, 0.04413116910601659615 ) ) ;
#341 = AXIS2_PLACEMENT_3D ( 'NONE', #20184, #3472, #18351 ) ;
#342 = EDGE_CURVE ( 'NONE', #14624, #11367, #6577, .T. ) ;
#343 = CARTESIAN_POINT ( 'NONE',  ( 0.3131180815194534173, 4.641677528921063889, -0.02196450506224391711 ) ) ;
#344 = CARTESIAN_POINT ( 'NONE',  ( 0.3155070326520292845, -5.795770164686806123E-17, -0.1286805555555552150 ) ) ;
#345 = B_SPLINE_CURVE_WITH_KNOTS ( 'NONE', 3,
 ( #21694, #10489, #23503, #6818, #14260, #4977 ),
 .UNSPECIFIED., .F., .F.,
 ( 4, 2, 4 ),
 ( 0.000000000000000000, 0.0002551367231383054124, 0.0005102734462766108248 ),
 .UNSPECIFIED. ) ;
#346 = CARTESIAN_POINT ( 'NONE',  ( 0.3119529355813799310, 4.306505973446880020, 0.04122820550216244745 ) ) ;
#347 = CARTESIAN_POINT ( 'NONE',  ( 0.1344534248014218336, 5.134761163306762910, 0.2754137591327791013 ) ) ;
#348 = EDGE_LOOP ( 'NONE', ( #13704, #13616, #8362, #11968, #22860, #19781, #8020, #11715 ) ) ;
#349 = CARTESIAN_POINT ( 'NONE',  ( 0.2923287055106771337, 0.07232142847388615958, -0.2123892367102620249 ) ) ;
#350 = CARTESIAN_POINT ( 'NONE',  ( 0.1993543840281266355, 0.5840277777019111660, 0.1993543840281267465 ) ) ;
#351 = CARTESIAN_POINT ( 'NONE',  ( 0.1144950937579611444, 0.2764156081756483641, -0.08874999999999956535 ) ) ;
#352 = CARTESIAN_POINT ( 'NONE',  ( 0.2869031291000053718, 0.6010169215856763225, -1.093172027866466278 ) ) ;
#353 = CARTESIAN_POINT ( 'NONE',  ( 0.08325293014416497439, 0.4931997757357156065, 0.4003306813560891242 ) ) ;
#354 = CARTESIAN_POINT ( 'NONE',  ( 0.2764156081756483641, 0.1144950937579610056, 0.1265277777777799595 ) ) ;
#355 = DIRECTION ( 'NONE',  ( 0.000000000000000000, 0.000000000000000000, -1.000000000000000000 ) ) ;
#356 = CARTESIAN_POINT ( 'NONE',  ( -4.638126268221291196E-16, 0.1232142855192009251, -0.4000000000000000222 ) ) ;
#357 = CARTESIAN_POINT ( 'NONE',  ( 1.910449006669871087E-17, 0.1986111111111107386, -0.3119999999999999996 ) ) ;
#358 = CARTESIAN_POINT ( 'NONE',  ( -0.3119999999999999996, 5.213972222222221120, -0.1292346314604056468 ) ) ;
#359 = VECTOR ( 'NONE', #7584, 39.37007874015748143 ) ;
#360 = CARTESIAN_POINT ( 'NONE',  ( -0.2819296736111110424, 4.148000000075866112, 0.1167790944451424923 ) ) ;
#361 = CARTESIAN_POINT ( 'NONE',  ( -0.2493918854782433692, 4.341271243197787122, 0.1918690073863245360 ) ) ;
#362 = FACE_OUTER_BOUND ( 'NONE', #13312, .T. ) ;
#363 = VERTEX_POINT ( 'NONE', #13911 ) ;
#364 = ADVANCED_FACE ( 'NONE', ( #12213 ), #623, .T. ) ;
#365 = CARTESIAN_POINT ( 'NONE',  ( 0.3236067977499789694, 0.3124999998049152183, 0.2351141009169893659 ) ) ;
#366 = CARTESIAN_POINT ( 'NONE',  ( -0.1167790944451423257, 4.953555555631421470, -0.2819296736111110424 ) ) ;
#367 = CARTESIAN_POINT ( 'NONE',  ( 0.05485615681475830563, -0.5228774440028900461, 0.05347937985141015815 ) ) ;
#368 = CARTESIAN_POINT ( 'NONE',  ( -0.3009367667953548597, 5.155896567499441474, 0.01723797010695745854 ) ) ;
#369 = EDGE_CURVE ( 'NONE', #17235, #19258, #1125, .T. ) ;
#370 = DIRECTION ( 'NONE',  ( -0.9690795681160667696, 0.000000000000000000, 0.2467484359828400198 ) ) ;
#371 = CARTESIAN_POINT ( 'NONE',  ( 8.973317209400627124E-05, 3.710497589222864434, -0.3120000002591014066 ) ) ;
#372 = CARTESIAN_POINT ( 'NONE',  ( 0.1954553509668046640, -0.1954553509668047195, -0.1130555555555552844 ) ) ;
#373 = AXIS2_PLACEMENT_3D ( 'NONE', #16147, #5038, #21752 ) ;
#374 = CARTESIAN_POINT ( 'NONE',  ( 0.1993543840281267465, 4.387583333409199149, 0.1993543840281266633 ) ) ;
#375 = DATE_TIME_ROLE ( 'classification_date' ) ;
#376 = CARTESIAN_POINT ( 'NONE',  ( -1.493307031895086562E-17, 0.4635611116728546865, -1.084197934689580034 ) ) ;
#377 = CARTESIAN_POINT ( 'NONE',  ( 0.2764156081756483641, -0.1144950937579611028, 0.008472222222223454655 ) ) ;
#378 = CARTESIAN_POINT ( 'NONE',  ( 0.2819296736111110424, 0.4902777777019112215, 0.1167790944451424923 ) ) ;
#379 = CARTESIAN_POINT ( 'NONE',  ( 0.1167790944451423257, 0.5597222221463555858, -0.2819296736111110424 ) ) ;
#380 = CARTESIAN_POINT ( 'NONE',  ( -0.09435543239133792337, 4.559812086079793048, -2.854670964936879329 ) ) ;
#381 = CARTESIAN_POINT ( 'NONE',  ( -0.3125000000000000000, 0.000000000000000000, 1.326383476483184332 ) ) ;
#382 = CARTESIAN_POINT ( 'NONE',  ( 0.1236067977499789028, 0.1714285714285714024, 0.3804226065180614791 ) ) ;
#383 = CARTESIAN_POINT ( 'NONE',  ( -3.863846776457871776E-17, -0.3155070326520292845, 0.1317361111111131078 ) ) ;
#384 = CARTESIAN_POINT ( 'NONE',  ( 0.4687500000000003886, 0.1745743740738040783, 0.4003190680884846642 ) ) ;
#385 = EDGE_CURVE ( 'NONE', #4141, #5067, #8524, .T. ) ;
#386 = CARTESIAN_POINT ( 'NONE',  ( -0.2782766723721450952, -0.03026958819837442111, -0.06867859833352769894 ) ) ;
#387 = CARTESIAN_POINT ( 'NONE',  ( 0.1167790944451423535, 0.4694444443685777957, 0.2819296736111110979 ) ) ;
#388 = CARTESIAN_POINT ( 'NONE',  ( -0.2819296736111110979, 0.1743055554796889284, -3.452642723725051716E-17 ) ) ;
#389 = ORIENTED_EDGE ( 'NONE', *, *, #20656, .T. ) ;
#390 = CARTESIAN_POINT ( 'NONE',  ( -0.2819296736111110424, 4.370222222298088433, 0.1167790944451424923 ) ) ;
#391 = CARTESIAN_POINT ( 'NONE',  ( -0.2472135954999579444, 0.4160714283763436994, -0.3402603233408159622 ) ) ;
#392 = CARTESIAN_POINT ( 'NONE',  ( -0.1167790944451423535, 4.932722222298088433, 0.2819296736111110424 ) ) ;
#393 = CARTESIAN_POINT ( 'NONE',  ( 0.2819296736111110979, 4.550777777853643791, -0.1167790944451423396 ) ) ;
#394 = AXIS2_PLACEMENT_3D ( 'NONE', #2859, #230, #22418 ) ;
#395 = CARTESIAN_POINT ( 'NONE',  ( 3.062437355670495042E-17, 0.4202679491924311561, -0.2499999999999999722 ) ) ;
#396 = AXIS2_PLACEMENT_3D ( 'NONE', #11256, #143, #18802 ) ;
#397 = VERTEX_POINT ( 'NONE', #8282 ) ;
#398 = DIRECTION ( 'NONE',  ( -1.000000000000000000, 0.000000000000000000, 0.000000000000000000 ) ) ;
#399 = CARTESIAN_POINT ( 'NONE',  ( -0.2206173157302028232, 3.995222222373953969, -0.2206173157302028232 ) ) ;
#400 = CARTESIAN_POINT ( 'NONE',  ( 1.910449006669871087E-17, 0.1430555555555552139, -0.3119999999999999996 ) ) ;
#401 = CARTESIAN_POINT ( 'NONE',  ( 0.05000000000000028727, 2.740000000000000213, -0.9255073213098983231 ) ) ;
#402 = EDGE_LOOP ( 'NONE', ( #17001, #2878, #11780, #16230 ) ) ;
#403 = COORDINATED_UNIVERSAL_TIME_OFFSET ( 0, 0, .AHEAD. ) ;
#404 = VERTEX_POINT ( 'NONE', #21099 ) ;
#405 = CARTESIAN_POINT ( 'NONE',  ( 0.08610082984204511791, 0.2741627315343106996, 0.3988756756980814111 ) ) ;
#406 = CIRCLE ( 'NONE', #20276, 0.001000000000000003057 ) ;
#407 = CYLINDRICAL_SURFACE ( 'NONE', #2541, 0.3125000000000000000 ) ;
#408 = CARTESIAN_POINT ( 'NONE',  ( -0.5116234456863258950, 2.853030769935284816, -2.640781157734872320 ) ) ;
#409 = VERTEX_POINT ( 'NONE', #19265 ) ;
#410 = CARTESIAN_POINT ( 'NONE',  ( -0.3119999999999999996, 0.4833333331816003775, -3.820898013339742174E-17 ) ) ;
#411 = VECTOR ( 'NONE', #12252, 39.37007874015748143 ) ;
#412 = VERTEX_POINT ( 'NONE', #6339 ) ;
#413 = CARTESIAN_POINT ( 'NONE',  ( 3.820898013339742174E-17, 5.384999999999999787, 0.3119999999999999996 ) ) ;
#414 = DIRECTION ( 'NONE',  ( -0.000000000000000000, -1.000000000000000000, -0.000000000000000000 ) ) ;
#415 = CARTESIAN_POINT ( 'NONE',  ( -0.3119999999999999996, 0.5423611111111107386, -0.1292346314604056745 ) ) ;
#416 = CARTESIAN_POINT ( 'NONE',  ( 0.2233192592356399164, 0.1258928570453146933, 0.3073725909049500604 ) ) ;
#417 = CARTESIAN_POINT ( 'NONE',  ( 0.1469174392757871539, 5.171225737096911246, 0.2578308252673338630 ) ) ;
#418 = ORIENTED_EDGE ( 'NONE', *, *, #12814, .T. ) ;
#419 = CARTESIAN_POINT ( 'NONE',  ( 0.3613381517857143232, 0.2973214284738861513, 0.000000000000000000 ) ) ;
#420 = DIRECTION ( 'NONE',  ( -0.8651979924482658957, 0.04370253788966848435, 0.4995222938423194425 ) ) ;
#421 = CARTESIAN_POINT ( 'NONE',  ( 0.2764156081756484196, -5.077672346800151106E-17, 0.4494444444444492537 ) ) ;
#422 = CARTESIAN_POINT ( 'NONE',  ( 0.1993543840281266633, 4.054250000075865223, -0.1993543840281266910 ) ) ;
#423 = DIRECTION ( 'NONE',  ( 0.000000000000000000, 0.000000000000000000, -1.000000000000000000 ) ) ;
#424 = CARTESIAN_POINT ( 'NONE',  ( 0.4593750000000003664, -0.2760455974562899817, 0.3779506566538943235 ) ) ;
#425 = CARTESIAN_POINT ( 'NONE',  ( -0.4500000000000003997, 0.2598076211353315679, 0.3779506566538943235 ) ) ;
#426 = CARTESIAN_POINT ( 'NONE',  ( -0.3119999999999999996, 4.668833333485065573, 0.000000000000000000 ) ) ;
#427 = CARTESIAN_POINT ( 'NONE',  ( -1.726321361862525858E-17, 5.019527777853643791, -0.2819296736111110979 ) ) ;
#428 = VERTEX_POINT ( 'NONE', #21220 ) ;
#429 = VECTOR ( 'NONE', #13673, 39.37007874015748143 ) ;
#430 = CARTESIAN_POINT ( 'NONE',  ( -1.726321361862525858E-17, 4.283416666742532186, -0.2819296736111110979 ) ) ;
#431 = VERTEX_POINT ( 'NONE', #4509 ) ;
#432 = CARTESIAN_POINT ( 'NONE',  ( -0.1116596296178200276, 0.04374999990245760639, 0.3436530038418508792 ) ) ;
#433 = ADVANCED_FACE ( 'NONE', ( #11974 ), #14262, .T. ) ;
#434 = ORIENTED_EDGE ( 'NONE', *, *, #12786, .F. ) ;
#435 = ORIENTED_EDGE ( 'NONE', *, *, #5401, .F. ) ;
#436 = PERSON_AND_ORGANIZATION_ROLE ( 'creator' ) ;
#437 =( BOUNDED_CURVE ( )  B_SPLINE_CURVE ( 2, ( #13480, #7963, #15531, #17360, #652, #13716, #4550, #12013, #19425 ),
 .UNSPECIFIED., .F., .F. ) 
 B_SPLINE_CURVE_WITH_KNOTS ( ( 3, 2, 2, 2, 3 ),
 ( 0.2000000000000000111, 0.2142857142857142738, 0.2285714285714285643, 0.2428571428571428548, 0.2500000000000000000 ),
 .UNSPECIFIED. ) 
 CURVE ( )  GEOMETRIC_REPRESENTATION_ITEM ( )  RATIONAL_B_SPLINE_CURVE ( ( 1.000000000000000000, 0.9510565162951535312, 1.000000000000000000, 0.9510565162951535312, 1.000000000000000000, 0.9510565162951535312, 1.000000000000000000, 0.9755282581475767101, 0.9755282581475768211 ) ) 
 REPRESENTATION_ITEM ( '' )  );
#438 = DIRECTION ( 'NONE',  ( 0.000000000000000000, 0.000000000000000000, -1.000000000000000000 ) ) ;
#439 = DIRECTION ( 'NONE',  ( 0.000000000000000000, 0.000000000000000000, 1.000000000000000000 ) ) ;
#440 = CARTESIAN_POINT ( 'NONE',  ( -0.1167790944451423119, 3.856333333409199149, -0.2819296736111110979 ) ) ;
#441 = CARTESIAN_POINT ( 'NONE',  ( 0.1058512031593883823, 4.429673085808546240, -0.2934957001599620141 ) ) ;
#442 = CARTESIAN_POINT ( 'NONE',  ( 0.2206173157302027954, 4.641055555555554157, -0.2206173157302028232 ) ) ;
#443 = LINE ( 'NONE', #11554, #17647 ) ;
#444 = CARTESIAN_POINT ( 'NONE',  ( 0.2764156081756483641, 0.1144950937579610195, 0.2862500000000035572 ) ) ;
#445 = CARTESIAN_POINT ( 'NONE',  ( 0.2819296736111110979, 0.5527777777019112770, -0.1167790944451422980 ) ) ;
#446 = CARTESIAN_POINT ( 'NONE',  ( 0.000000000000000000, 0.2764156081756484196, -0.09222222222222178911 ) ) ;
#447 = ORIENTED_EDGE ( 'NONE', *, *, #19474, .T. ) ;
#448 = CARTESIAN_POINT ( 'NONE',  ( 0.1993543840281266633, 4.734805555631421470, -0.1993543840281266910 ) ) ;
#449 = CARTESIAN_POINT ( 'NONE',  ( 0.006583558500310691085, -0.5374648580928945707, 0.05971062996525675765 ) ) ;
#450 = CARTESIAN_POINT ( 'NONE',  ( -0.1167790944451423257, 4.731333333409198261, -0.2819296736111110424 ) ) ;
#451 = CARTESIAN_POINT ( 'NONE',  ( -0.1458082941847503033, 0.2460910087212002384, -0.07505195856086301076 ) ) ;
#452 = CARTESIAN_POINT ( 'NONE',  ( 0.2588148980552389400, 4.857971016408025200, 0.1753205476218995251 ) ) ;
#453 = CARTESIAN_POINT ( 'NONE',  ( -0.1385944955600183770, -6.721771644360946285E-18, 0.3536177551490795046 ) ) ;
#454 = CARTESIAN_POINT ( 'NONE',  ( 0.2195630361086305937, -0.1679215936616662852, 0.3880822748423153334 ) ) ;
#455 = CARTESIAN_POINT ( 'NONE',  ( -0.2206173157302028232, 4.488277777777776478, -0.2206173157302028232 ) ) ;
#456 = CARTESIAN_POINT ( 'NONE',  ( -0.2819296736111110979, 3.793833333409199149, -0.1167790944451422980 ) ) ;
#457 = CARTESIAN_POINT ( 'NONE',  ( -0.1292346314604106428, 4.005638888888888083, 0.3119999999999950036 ) ) ;
#458 = CC_DESIGN_PERSON_AND_ORGANIZATION_ASSIGNMENT ( #23571, #12269, ( #8791 ) ) ;
#459 = ORIENTED_EDGE ( 'NONE', *, *, #15967, .F. ) ;
#460 = CARTESIAN_POINT ( 'NONE',  ( 0.000000000000000000, 5.580000000000000959, -0.2500000000000000555 ) ) ;
#461 = ORIENTED_EDGE ( 'NONE', *, *, #3849, .T. ) ;
#462 = CARTESIAN_POINT ( 'NONE',  ( 0.3118815705390921011, 4.695382381602317245, 0.04185132024466815120 ) ) ;
#463 = CARTESIAN_POINT ( 'NONE',  ( 3.887228417612631703E-07, 4.154944433789834690, -0.3119999999997578044 ) ) ;
#464 = CARTESIAN_POINT ( 'NONE',  ( 0.1954553509668046640, -0.1954553509668047195, 0.4425000000000047229 ) ) ;
#465 = DIRECTION ( 'NONE',  ( -1.000000000000000000, 0.000000000000000000, 0.000000000000000000 ) ) ;
#466 = ORIENTED_EDGE ( 'NONE', *, *, #1277, .F. ) ;
#467 = EDGE_CURVE ( 'NONE', #10173, #22264, #19322, .T. ) ;
#468 = CARTESIAN_POINT ( 'NONE',  ( -6.979263641208234666E-17, -0.02410714295468524906, 0.3799334167787516425 ) ) ;
#469 = CARTESIAN_POINT ( 'NONE',  ( 0.2819296736111110424, 0.4277777777019111105, -0.1167790944451423119 ) ) ;
#470 = LINE ( 'NONE', #15474, #5473 ) ;
#471 = CARTESIAN_POINT ( 'NONE',  ( 3.820898013339742174E-17, 5.384999999999999787, 0.3119999999999999996 ) ) ;
#472 = CARTESIAN_POINT ( 'NONE',  ( 1.910449006669871087E-17, 0.1430555555555552139, -0.3119999999999999996 ) ) ;
#473 = CARTESIAN_POINT ( 'NONE',  ( 0.1954553509668046640, -0.1954553509668047195, 0.1161111111111132049 ) ) ;
#474 = CARTESIAN_POINT ( 'NONE',  ( -0.2361897315408544862, 4.619585270958687317, 0.2066264843407155938 ) ) ;
#475 = CARTESIAN_POINT ( 'NONE',  ( 1.910449006669871087E-17, 0.08749999999999966138, -0.3119999999999999996 ) ) ;
#476 = CARTESIAN_POINT ( 'NONE',  ( 0.4901945818292207657, 2.760194581829221061, -0.07019458182922092004 ) ) ;
#477 = CARTESIAN_POINT ( 'NONE',  ( 1.910449006669871087E-17, 0.3097222222222218435, -0.3119999999999999996 ) ) ;
#478 = CARTESIAN_POINT ( 'NONE',  ( -0.3119999999999999996, 5.106333333333332725, 0.000000000000000000 ) ) ;
#479 = EDGE_CURVE ( 'NONE', #5967, #549, #1001, .T. ) ;
#480 = CARTESIAN_POINT ( 'NONE',  ( 0.1167790944451422702, 4.127166666742532186, -0.2819296736111110424 ) ) ;
#481 = CARTESIAN_POINT ( 'NONE',  ( -0.1571792371097448515, 4.326278488575934666, -0.2725945807372967544 ) ) ;
#482 = DIRECTION ( 'NONE',  ( 0.000000000000000000, 1.000000000000000000, 0.000000000000000000 ) ) ;
#483 = CARTESIAN_POINT ( 'NONE',  ( 0.06335377612981493711, 0.3750447955744454220, 0.3999999999999999667 ) ) ;
#484 = ORIENTED_EDGE ( 'NONE', *, *, #13372, .F. ) ;
#485 = CARTESIAN_POINT ( 'NONE',  ( 0.06335377612981453466, 0.3356694897496707020, -0.3999999999999999667 ) ) ;
#486 = CARTESIAN_POINT ( 'NONE',  ( -0.2819296736111110424, 4.800777777853643791, 0.1167790944451424923 ) ) ;
#487 = AXIS2_PLACEMENT_3D ( 'NONE', #15948, #3030, #21441 ) ;
#488 = CARTESIAN_POINT ( 'NONE',  ( 0.01172578639831932910, 0.5344959914317446437, 0.04874733047933995506 ) ) ;
#489 = CARTESIAN_POINT ( 'NONE',  ( -0.02861657392953457710, 4.515272125417114424, 0.3106861733379689405 ) ) ;
#490 = CARTESIAN_POINT ( 'NONE',  ( 0.4805070082343983473, -0.2560807851245830435, 0.04413116910601658921 ) ) ;
#491 = CARTESIAN_POINT ( 'NONE',  ( 0.3119999999999998885, 0.6187499998482670627, 0.1292346314604058410 ) ) ;
#492 = CARTESIAN_POINT ( 'NONE',  ( 0.1167790944451424506, 4.217444444520309865, 0.2819296736111110424 ) ) ;
#493 = DATE_AND_TIME ( #11482, #21662 ) ;
#494 = CARTESIAN_POINT ( 'NONE',  ( -0.2031932902514208272, 4.050132635743126208, -0.2367657278459141534 ) ) ;
#495 = CARTESIAN_POINT ( 'NONE',  ( 0.000000000000000000, 0.2764156081756484196, -0.02972222222222129645 ) ) ;
#496 = ORIENTED_EDGE ( 'NONE', *, *, #14555, .F. ) ;
#497 = CARTESIAN_POINT ( 'NONE',  ( 0.2819296736111110424, 0.4416666665908000056, -0.1167790944451423119 ) ) ;
#498 = DIRECTION ( 'NONE',  ( -0.000000000000000000, -0.000000000000000000, -1.000000000000000000 ) ) ;
#499 = CARTESIAN_POINT ( 'NONE',  ( 4.375590819076689459E-17, 0.01607142837634377430, 0.4000000000000000222 ) ) ;
#500 = CARTESIAN_POINT ( 'NONE',  ( -0.1236067977499790416, 0.3071428571428570509, 0.3804226065180614236 ) ) ;
#501 = CARTESIAN_POINT ( 'NONE',  ( 0.3155070326520292290, 0.1306872919485615736, 0.2046527777777804036 ) ) ;
#502 = CIRCLE ( 'NONE', #21150, 0.3125000000000000000 ) ;
#503 = CARTESIAN_POINT ( 'NONE',  ( 0.3125000000000000000, -5.740531871003217465E-17, 0.03277777777777902274 ) ) ;
#504 = CARTESIAN_POINT ( 'NONE',  ( 2.911000000000000032, 0.04999999999999919092, 0.000000000000000000 ) ) ;
#505 = CARTESIAN_POINT ( 'NONE',  ( -5.178964085587577574E-17, 0.5215277777019111660, 0.2819296736111110979 ) ) ;
#506 = CARTESIAN_POINT ( 'NONE',  ( 0.2819296736111110424, 0.1430555554796889284, 0.1167790944451424923 ) ) ;
#507 = CARTESIAN_POINT ( 'NONE',  ( 0.1167790944451424368, 4.384111111186976828, 0.2819296736111110424 ) ) ;
#508 = CARTESIAN_POINT ( 'NONE',  ( -0.2472135954999579444, 0.2017857140906294255, -0.3402603233408159622 ) ) ;
#509 = ADVANCED_FACE ( 'NONE', ( #18279 ), #1216, .F. ) ;
#510 = CARTESIAN_POINT ( 'NONE',  ( -0.1167790944451423257, 4.800777777853643791, -0.2819296736111110424 ) ) ;
#511 = CARTESIAN_POINT ( 'NONE',  ( 5.178964085587577574E-17, 4.144527777853642903, 0.2819296736111110979 ) ) ;
#512 = CARTESIAN_POINT ( 'NONE',  ( 2.114711001306381011, 2.690000000000002167, -2.986000000000000210 ) ) ;
#513 = CARTESIAN_POINT ( 'NONE',  ( 0.2209708691207961095, -0.2209708691207961651, 0.2480555555555585268 ) ) ;
#514 = CARTESIAN_POINT ( 'NONE',  ( 0.2206173157302027954, 3.870222222373954413, -0.2206173157302028232 ) ) ;
#515 = DIRECTION ( 'NONE',  ( 0.000000000000000000, 0.000000000000000000, 1.000000000000000000 ) ) ;
#516 = VECTOR ( 'NONE', #6210, 39.37007874015748143 ) ;
#517 = CARTESIAN_POINT ( 'NONE',  ( 0.2774634594257791576, -0.1150700753240518487, -0.08907806777757856787 ) ) ;
#518 = ORIENTED_EDGE ( 'NONE', *, *, #538, .F. ) ;
#519 = PERSON_AND_ORGANIZATION ( #15518, #2538 ) ;
#520 = CARTESIAN_POINT ( 'NONE',  ( -0.3065849364905382513, 4.708020935245015622E-15, -0.09575160315720471216 ) ) ;
#521 = EDGE_CURVE ( 'NONE', #8592, #18897, #11168, .T. ) ;
#522 = CARTESIAN_POINT ( 'NONE',  ( -0.2740748391469606249, 5.006672122428321714, 0.1502628184871280526 ) ) ;
#523 = ORIENTED_EDGE ( 'NONE', *, *, #20352, .F. ) ;
#524 = CARTESIAN_POINT ( 'NONE',  ( 1.726321361862525858E-17, 0.06319444436857780956, -0.2819296736111110979 ) ) ;
#525 = EDGE_CURVE ( 'NONE', #11560, #14350, #13656, .T. ) ;
#526 = ADVANCED_FACE ( 'NONE', ( #16455 ), #6821, .T. ) ;
#527 = ORIENTED_EDGE ( 'NONE', *, *, #15962, .T. ) ;
#528 = DIRECTION ( 'NONE',  ( -0.000000000000000000, 1.000000000000000000, -0.000000000000000000 ) ) ;
#529 = CARTESIAN_POINT ( 'NONE',  ( 0.000000000000000000, 3.700000000000000622, 0.000000000000000000 ) ) ;
#530 = CARTESIAN_POINT ( 'NONE',  ( 0.002608860322658908878, 4.765981492550016796, -0.3119906577544150905 ) ) ;
#531 = CARTESIAN_POINT ( 'NONE',  ( 0.1116596296178199860, 0.1508928570453147155, -0.3436530038418508792 ) ) ;
#532 = CARTESIAN_POINT ( 'NONE',  ( 0.2898213196250513102, 5.180044785969154297, -0.04452301891601496975 ) ) ;
#533 = ORIENTED_EDGE ( 'NONE', *, *, #294, .F. ) ;
#534 = CARTESIAN_POINT ( 'NONE',  ( 0.2233192592356399164, 0.2866071427596003640, 0.3073725909049500604 ) ) ;
#535 = DIRECTION ( 'NONE',  ( 0.000000000000000000, 0.000000000000000000, 1.000000000000000000 ) ) ;
#536 = CARTESIAN_POINT ( 'NONE',  ( -0.3119999999999998885, 4.054249999999999687, 0.1292346314604058410 ) ) ;
#537 = VECTOR ( 'NONE', #2199, 39.37007874015748143 ) ;
#538 = EDGE_CURVE ( 'NONE', #12392, #3340, #18037, .T. ) ;
#539 = CARTESIAN_POINT ( 'NONE',  ( 0.1993543840281267465, 4.040361111186976828, 0.1993543840281266633 ) ) ;
#540 = CARTESIAN_POINT ( 'NONE',  ( 0.8352479138593175145, 0.000000000000000000, -3.011000000000000565 ) ) ;
#541 = CARTESIAN_POINT ( 'NONE',  ( 8.984713656453739555E-13, 5.162518060853549251, -0.2988821118451543968 ) ) ;
#542 = CARTESIAN_POINT ( 'NONE',  ( -0.1292346314604056745, 4.825083333485066461, -0.3119999999999999996 ) ) ;
#543 = CARTESIAN_POINT ( 'NONE',  ( -0.1167790944451423119, 4.967444444520310753, -0.2819296736111110979 ) ) ;
#544 = VERTEX_POINT ( 'NONE', #20232 ) ;
#545 = CARTESIAN_POINT ( 'NONE',  ( 0.1993543840281266633, 4.276472222298087544, -0.1993543840281266910 ) ) ;
#546 = EDGE_LOOP ( 'NONE', ( #12242, #17366, #3544, #9068 ) ) ;
#547 = CARTESIAN_POINT ( 'NONE',  ( 0.2233192592356399164, 0.1973214284738861179, 0.3073725909049500604 ) ) ;
#548 = ORIENTED_EDGE ( 'NONE', *, *, #15332, .T. ) ;
#549 = VERTEX_POINT ( 'NONE', #12692 ) ;
#550 = APPLICATION_PROTOCOL_DEFINITION ( 'international standard', 'config_control_design', 1994, #23355 ) ;
#551 = VECTOR ( 'NONE', #33, 39.37007874015748143 ) ;
#552 = FACE_OUTER_BOUND ( 'NONE', #3950, .T. ) ;
#553 = CARTESIAN_POINT ( 'NONE',  ( 0.3124999999999989453, 0.1294417382415933571, 0.2584722222222253230 ) ) ;
#554 = CARTESIAN_POINT ( 'NONE',  ( -0.3119999999999999996, 0.09791666651493373397, 0.1292346314604056190 ) ) ;
#555 = CARTESIAN_POINT ( 'NONE',  ( 0.1698237203583192467, 4.427710968560108817, -0.2637982107419344358 ) ) ;
#556 = CARTESIAN_POINT ( 'NONE',  ( -0.4687500000000002776, -0.1098280991662788780, 0.4107862666565998966 ) ) ;
#557 = LINE ( 'NONE', #17027, #4020 ) ;
#558 =( GEOMETRIC_REPRESENTATION_CONTEXT ( 3 ) GLOBAL_UNCERTAINTY_ASSIGNED_CONTEXT ( ( #11693 ) ) GLOBAL_UNIT_ASSIGNED_CONTEXT ( ( #9433, #22474, #11881 ) ) REPRESENTATION_CONTEXT ( 'NONE', 'WORKASPACE' ) );
#559 = CARTESIAN_POINT ( 'NONE',  ( -0.1954553509668046640, 0.1954553509668046918, 0.1369444444444467002 ) ) ;
#560 = CARTESIAN_POINT ( 'NONE',  ( -0.2819296736111110979, 0.4624999999241333759, -0.1167790944451423396 ) ) ;
#561 = CARTESIAN_POINT ( 'NONE',  ( 0.1954553509668046640, -0.1954553509668047195, 0.4494444444444491427 ) ) ;
#562 = EDGE_CURVE ( 'NONE', #15146, #13004, #700, .T. ) ;
#563 = EDGE_LOOP ( 'NONE', ( #5895, #19879, #20173, #15118 ) ) ;
#564 = CARTESIAN_POINT ( 'NONE',  ( -0.2819296736111110424, 4.641055555631422358, -0.1167790944451423119 ) ) ;
#565 = CARTESIAN_POINT ( 'NONE',  ( -0.2472135954999579444, 0.4160714283763437549, -0.3402603233408160732 ) ) ;
#566 = EDGE_CURVE ( 'NONE', #9581, #14200, #18166, .T. ) ;
#567 = CARTESIAN_POINT ( 'NONE',  ( 5.178964085587577574E-17, 4.644527777853642903, 0.2819296736111110979 ) ) ;
#568 = LINE ( 'NONE', #329, #15357 ) ;
#569 = CYLINDRICAL_SURFACE ( 'NONE', #13680, 0.3119999999999999996 ) ;
#570 = CARTESIAN_POINT ( 'NONE',  ( 0.3699999999999995515, 0.000000000000000000, -1.922698729810778273 ) ) ;
#571 = CARTESIAN_POINT ( 'NONE',  ( 1.682181019992768034, 2.405292355953585481, -2.038697013607245978 ) ) ;
#572 = CARTESIAN_POINT ( 'NONE',  ( 0.2206173157302027954, 4.252166666666665762, -0.2206173157302028232 ) ) ;
#573 = CARTESIAN_POINT ( 'NONE',  ( -0.2819296736111110979, 3.797305555631421470, 0.000000000000000000 ) ) ;
#574 = VECTOR ( 'NONE', #6340, 39.37007874015748143 ) ;
#575 = DIRECTION ( 'NONE',  ( -0.000000000000000000, -1.000000000000000000, -0.000000000000000000 ) ) ;
#576 = ORIENTED_EDGE ( 'NONE', *, *, #13809, .F. ) ;
#577 = DIMENSIONAL_EXPONENTS ( 1.000000000000000000, 0.000000000000000000, 0.000000000000000000, 0.000000000000000000, 0.000000000000000000, 0.000000000000000000, 0.000000000000000000 ) ;
#578 = CYLINDRICAL_SURFACE ( 'NONE', #9347, 0.4000000000000000222 ) ;
#579 = ORIENTED_EDGE ( 'NONE', *, *, #18990, .T. ) ;
#580 =( BOUNDED_CURVE ( )  B_SPLINE_CURVE ( 2, ( #15781, #4678, #899, #4561, #19800, #3097, #781, #8211, #8694 ),
 .UNSPECIFIED., .F., .T. ) 
 B_SPLINE_CURVE_WITH_KNOTS ( ( 3, 2, 2, 2, 3 ),
 ( 0.1041666666666666713, 0.1145833333333333287, 0.1250000000000000000, 0.1354166666666666574, 0.1458333333333333426 ),
 .UNSPECIFIED. ) 
 CURVE ( )  GEOMETRIC_REPRESENTATION_ITEM ( )  RATIONAL_B_SPLINE_CURVE ( ( 1.000000000000000000, 0.9238795325112867385, 1.000000000000000000, 0.9238795325112867385, 1.000000000000000000, 0.9238795325112867385, 1.000000000000000000, 0.9238795325112867385, 1.000000000000000000 ) ) 
 REPRESENTATION_ITEM ( '' )  );
#581 =( BOUNDED_CURVE ( )  B_SPLINE_CURVE ( 2, ( #7062, #19982, #3270, #7304, #10723, #20106, #16572, #22169, #3395 ),
 .UNSPECIFIED., .F., .F. ) 
 B_SPLINE_CURVE_WITH_KNOTS ( ( 3, 2, 2, 2, 3 ),
 ( 0.3541666666666666852, 0.3645833333333333703, 0.3750000000000000555, 0.3854166666666667407, 0.3958333333333334259 ),
 .UNSPECIFIED. ) 
 CURVE ( )  GEOMETRIC_REPRESENTATION_ITEM ( )  RATIONAL_B_SPLINE_CURVE ( ( 1.000000000000000000, 0.9238795325112867385, 1.000000000000000000, 0.9238795325112867385, 1.000000000000000000, 0.9238795325112867385, 1.000000000000000000, 0.9238795325112859613, 1.000000000000000888 ) ) 
 REPRESENTATION_ITEM ( '' )  );
#582 = PRODUCT_DEFINITION_FORMATION_WITH_SPECIFIED_SOURCE ( 'ANY', '', #12267, .NOT_KNOWN. ) ;
#583 = CARTESIAN_POINT ( 'NONE',  ( 0.3035962428291631987, 4.694232598334442841, 0.08277057684829301765 ) ) ;
#584 = SPHERICAL_SURFACE ( 'NONE', #1430, 0.01874999999999999931 ) ;
#585 = CARTESIAN_POINT ( 'NONE',  ( 0.3155070326520292290, 0.1306872919485615736, -0.1252083333333329496 ) ) ;
#586 = VECTOR ( 'NONE', #16991, 39.37007874015748143 ) ;
#587 = CARTESIAN_POINT ( 'NONE',  ( 0.1914943533321577518, 4.299605383836522243, 0.2496738231090171456 ) ) ;
#588 = EDGE_LOOP ( 'NONE', ( #11742, #10987, #11274, #3654 ) ) ;
#589 = CARTESIAN_POINT ( 'NONE',  ( -0.2923287055106771337, -0.04910714295468524004, -0.2123892367102620804 ) ) ;
#590 = CARTESIAN_POINT ( 'NONE',  ( -0.1167790944451422702, 0.4416666665908000611, -0.2819296736111110424 ) ) ;
#591 = CARTESIAN_POINT ( 'NONE',  ( -0.1048218097661234444, 5.206640035683669510, 0.2619026841321052124 ) ) ;
#592 = CARTESIAN_POINT ( 'NONE',  ( 0.02089524249861754446, 0.7885332705621130867, -1.079944001585411817 ) ) ;
#593 = CARTESIAN_POINT ( 'NONE',  ( -0.2107770390571470920, -0.2008625216908039579, -0.07979188311515521270 ) ) ;
#594 = CARTESIAN_POINT ( 'NONE',  ( -0.1954553509668046918, -0.1954553509668046640, 0.2133333333333361503 ) ) ;
#595 = ORIENTED_EDGE ( 'NONE', *, *, #6816, .T. ) ;
#596 = CARTESIAN_POINT ( 'NONE',  ( -0.1635002882892696296, 4.622259302225510069, 0.2657784613148136410 ) ) ;
#597 = DIRECTION ( 'NONE',  ( 0.000000000000000000, 0.000000000000000000, 1.000000000000000000 ) ) ;
#598 = LOCAL_TIME ( 21, 9, 13.00000000000000000, #9467 ) ;
#599 = CARTESIAN_POINT ( 'NONE',  ( 0.2752577204847949655, 1.857579423845309578E-17, -0.2411543459231450526 ) ) ;
#600 = CARTESIAN_POINT ( 'NONE',  ( -5.731347020009612645E-17, 0.1708333333333330040, 0.3119999999999999996 ) ) ;
#601 = CARTESIAN_POINT ( 'NONE',  ( 0.2206173157302027954, 4.974388888888888083, -0.2206173157302028232 ) ) ;
#602 = CARTESIAN_POINT ( 'NONE',  ( -0.1993543840281266355, 4.095916666742533074, 0.1993543840281267465 ) ) ;
#603 = FACE_OUTER_BOUND ( 'NONE', #11639, .T. ) ;
#604 = LINE ( 'NONE', #22912, #21836 ) ;
#605 = DIRECTION ( 'NONE',  ( 0.000000000000000000, 1.000000000000000000, 0.000000000000000000 ) ) ;
#606 = VERTEX_POINT ( 'NONE', #6943 ) ;
#607 = ORIENTED_EDGE ( 'NONE', *, *, #85, .F. ) ;
#608 = CARTESIAN_POINT ( 'NONE',  ( 0.2998642343065497373, 0.08796414601275419354, 0.4241666666666771834 ) ) ;
#609 = CARTESIAN_POINT ( 'NONE',  ( 0.2819296736111110424, 4.773000000075865223, -0.1167790944451423396 ) ) ;
#610 = CIRCLE ( 'NONE', #7625, 0.3125000000000000000 ) ;
#611 = CARTESIAN_POINT ( 'NONE',  ( 0.2233192592356400275, 0.3616071427596003751, -0.3073725909049499494 ) ) ;
#612 = EDGE_CURVE ( 'NONE', #20185, #20917, #15444, .T. ) ;
#613 = CARTESIAN_POINT ( 'NONE',  ( 5.463034709641816805E-17, 5.167344860100310910, 0.2973937581265823082 ) ) ;
#614 = APPROVAL_STATUS ( 'not_yet_approved' ) ;
#615 = CARTESIAN_POINT ( 'NONE',  ( -1.856450067443490846E-16, 0.5196152422706634688, 0.3779506566538943790 ) ) ;
#616 = CARTESIAN_POINT ( 'NONE',  ( 0.3119999999999999996, 0.6222222220704892726, 0.000000000000000000 ) ) ;
#617 = LOCAL_TIME ( 21, 9, 13.00000000000000000, #22571 ) ;
#618 = CARTESIAN_POINT ( 'NONE',  ( 0.1167790944451422702, 4.349388888964754507, -0.2819296736111110979 ) ) ;
#619 = APPROVAL ( #20860, 'UNKNOWN' ) ;
#620 = EDGE_CURVE ( 'NONE', #3437, #18019, #10851, .T. ) ;
#621 = CARTESIAN_POINT ( 'NONE',  ( -0.09435543239133792337, 1.041821957232212270, -2.854670964936879329 ) ) ;
#622 = DIRECTION ( 'NONE',  ( -0.000000000000000000, 1.000000000000000000, -0.000000000000000000 ) ) ;
#623 = CONICAL_SURFACE ( 'NONE', #17373, 1.243000000000000105, 0.7853981633974551624 ) ;
#624 = CARTESIAN_POINT ( 'NONE',  ( -0.2819296736111110979, 0.3583333332574666907, 0.1167790944451422425 ) ) ;
#625 = CARTESIAN_POINT ( 'NONE',  ( 4.282505654011733572E-07, 3.932722210548942776, -0.3119999999997061790 ) ) ;
#626 = CARTESIAN_POINT ( 'NONE',  ( -0.3236067977499789694, 0.1428571428571428215, -0.2351141009169893104 ) ) ;
#627 = CARTESIAN_POINT ( 'NONE',  ( -0.1060554323913378977, 4.559812086079793048, -2.874935959385435336 ) ) ;
#628 = CARTESIAN_POINT ( 'NONE',  ( 0.2230971623002953874, -0.2230971623002954429, 0.1386805555555576386 ) ) ;
#629 = CARTESIAN_POINT ( 'NONE',  ( 0.3119999999999999996, 3.970916666666665318, -0.1292346314604056745 ) ) ;
#630 = CARTESIAN_POINT ( 'NONE',  ( 0.2206173157302028787, 5.016055555555554157, 0.2206173157302027954 ) ) ;
#631 = CARTESIAN_POINT ( 'NONE',  ( -0.2819296736111110979, 0.5597222221463555858, -0.1167790944451423396 ) ) ;
#632 = CARTESIAN_POINT ( 'NONE',  ( -0.2819296736111110424, 0.2819444443685777957, -0.1167790944451423396 ) ) ;
#633 = CARTESIAN_POINT ( 'NONE',  ( -0.1993543840281266355, 4.207027777853643791, 0.1993543840281267465 ) ) ;
#634 = CARTESIAN_POINT ( 'NONE',  ( -0.3236067977499789694, 0.2767857140906295199, -0.2351141009169893104 ) ) ;
#635 = CARTESIAN_POINT ( 'NONE',  ( -0.1167790944451423257, 4.856333333409199149, -0.2819296736111110424 ) ) ;
#636 = PLANE ( 'NONE',  #7128 ) ;
#637 = LOCAL_TIME ( 21, 9, 13.00000000000000000, #6099 ) ;
#638 = ORIENTED_EDGE ( 'NONE', *, *, #2660, .F. ) ;
#639 = DIRECTION ( 'NONE',  ( 0.6399207742898923579, 0.6399207742898924689, -0.4254442446013919077 ) ) ;
#640 = CARTESIAN_POINT ( 'NONE',  ( 0.2206173157302028787, 3.745222222373954413, 0.2206173157302027954 ) ) ;
#641 = CARTESIAN_POINT ( 'NONE',  ( -0.009375000000000190473, 0.5358532185916217161, 0.3779506566538943790 ) ) ;
#642 = VECTOR ( 'NONE', #11209, 39.37007874015748143 ) ;
#643 = EDGE_CURVE ( 'NONE', #17766, #11636, #18399, .T. ) ;
#644 = VERTEX_POINT ( 'NONE', #18759 ) ;
#645 = CALENDAR_DATE ( 2026, 7, 10 ) ;
#646 = EDGE_CURVE ( 'NONE', #2198, #7226, #16693, .T. ) ;
#647 = CARTESIAN_POINT ( 'NONE',  ( 0.06335377612981493711, 0.3125447957695302037, 0.3999999999999999667 ) ) ;
#648 = CARTESIAN_POINT ( 'NONE',  ( -0.2300939842550158432, 5.008739598255579573, 0.2107150241362776288 ) ) ;
#649 = EDGE_LOOP ( 'NONE', ( #2562, #20892, #11863, #14301 ) ) ;
#650 = CARTESIAN_POINT ( 'NONE',  ( -0.1167790944451424368, 0.1430555554796889284, 0.2819296736111110424 ) ) ;
#651 = ORIENTED_EDGE ( 'NONE', *, *, #19743, .T. ) ;
#652 = CARTESIAN_POINT ( 'NONE',  ( -0.3236067977499790249, 0.01428571428571426098, 0.2351141009169892271 ) ) ;
#653 = CARTESIAN_POINT ( 'NONE',  ( 0.07411063262685617381, 0.4869405031891889668, 0.4162703459413902851 ) ) ;
#654 = FACE_OUTER_BOUND ( 'NONE', #10954, .T. ) ;
#655 = CARTESIAN_POINT ( 'NONE',  ( 0.1116596296178199860, 0.2937499999024575925, -0.3436530038418508792 ) ) ;
#656 = CARTESIAN_POINT ( 'NONE',  ( 0.03852464118876493954, 5.189404391384640824, -0.2870586899848421303 ) ) ;
#657 = EDGE_LOOP ( 'NONE', ( #12785, #23808, #23001, #6028, #16754 ) ) ;
#658 = CARTESIAN_POINT ( 'NONE',  ( 0.000000000000000000, 0.9300000000000000488, 0.000000000000000000 ) ) ;
#659 = AXIS2_PLACEMENT_3D ( 'NONE', #4875, #17930, #1226 ) ;
#660 = CARTESIAN_POINT ( 'NONE',  ( -0.2499225477423614450, 4.674556910496129980, 0.1869683874588545791 ) ) ;
#661 = CARTESIAN_POINT ( 'NONE',  ( -0.1167790944451423257, 4.009111111186976828, -0.2819296736111110424 ) ) ;
#662 = CARTESIAN_POINT ( 'NONE',  ( 2.064578755398029967E-15, 5.043833333485014947, -0.3119999999999999996 ) ) ;
#663 = CARTESIAN_POINT ( 'NONE',  ( -0.07624758732758733781, 5.194631950919444741, 0.2776879540135884228 ) ) ;
#664 = CARTESIAN_POINT ( 'NONE',  ( 0.3119999999999999996, 4.422305555707287894, -0.1292346314604056745 ) ) ;
#665 = CARTESIAN_POINT ( 'NONE',  ( -0.1993543840281266910, 4.970916666742532186, -0.1993543840281266910 ) ) ;
#666 = EDGE_CURVE ( 'NONE', #787, #19238, #18451, .T. ) ;
#667 = ORIENTED_EDGE ( 'NONE', *, *, #19117, .F. ) ;
#668 = ADVANCED_FACE ( 'NONE', ( #22659 ), #20708, .F. ) ;
#669 = CARTESIAN_POINT ( 'NONE',  ( 0.2819296736111110424, 3.995222222298087544, -0.1167790944451423396 ) ) ;
#670 = EDGE_CURVE ( 'NONE', #23659, #6065, #12081, .T. ) ;
#671 = ORIENTED_EDGE ( 'NONE', *, *, #3179, .F. ) ;
#672 = CARTESIAN_POINT ( 'NONE',  ( -0.2923287055106771337, 0.2366071427596004584, -0.2123892367102620804 ) ) ;
#673 = ORIENTED_EDGE ( 'NONE', *, *, #14315, .T. ) ;
#674 = VECTOR ( 'NONE', #17420, 39.37007874015748143 ) ;
#675 = ORIENTED_EDGE ( 'NONE', *, *, #13849, .T. ) ;
#676 = PERSON_AND_ORGANIZATION ( #15518, #2538 ) ;
#677 = EDGE_CURVE ( 'NONE', #3460, #23837, #22893, .T. ) ;
#678 = ORIENTED_EDGE ( 'NONE', *, *, #19419, .T. ) ;
#679 = CARTESIAN_POINT ( 'NONE',  ( -0.3834923435458895136, -0.3083291687941427384, 0.4165495381634257144 ) ) ;
#680 = CARTESIAN_POINT ( 'NONE',  ( 0.2209708691207961651, 0.2209708691207959985, 0.2619444444444474773 ) ) ;
#681 = CARTESIAN_POINT ( 'NONE',  ( -0.3119999999999999996, 0.1465277776260448805, -0.1292346314604056745 ) ) ;
#682 = CARTESIAN_POINT ( 'NONE',  ( 0.07114610157022679959, 4.406947439583936088, 0.3037810326460302912 ) ) ;
#683 = DIRECTION ( 'NONE',  ( -0.8459207832372985791, 0.4883925919151526074, 0.2142211582677925885 ) ) ;
#684 = CARTESIAN_POINT ( 'NONE',  ( 0.05482159418621733449, -0.5228976771666083989, 0.05347049744908469182 ) ) ;
#685 = CARTESIAN_POINT ( 'NONE',  ( 0.1954553509668046640, -0.1954553509668047195, 0.1647222222222247123 ) ) ;
#686 = CARTESIAN_POINT ( 'NONE',  ( 0.1167790944451423535, 0.4833333332574666907, 0.2819296736111110979 ) ) ;
#687 = CARTESIAN_POINT ( 'NONE',  ( 0.000000000000000000, 0.2764156081756484196, 0.4147222222222267107 ) ) ;
#688 = ORIENTED_EDGE ( 'NONE', *, *, #165, .T. ) ;
#689 = CARTESIAN_POINT ( 'NONE',  ( 0.2819296736111110979, 4.724388888964754507, 0.1167790944451422425 ) ) ;
#690 = CARTESIAN_POINT ( 'NONE',  ( 0.9244709581221690620, 2.291712385858714285, -1.333428253224823168 ) ) ;
#691 = CARTESIAN_POINT ( 'NONE',  ( 0.2819296736111110424, 4.717444444520309865, -0.1167790944451423396 ) ) ;
#692 = CARTESIAN_POINT ( 'NONE',  ( 0.4582856249906270274, -0.2428769834202093303, 0.4003459333743809578 ) ) ;
#693 = CARTESIAN_POINT ( 'NONE',  ( 0.2906999326536478523, 4.866559060925098379, -0.1133051895180592905 ) ) ;
#694 = CARTESIAN_POINT ( 'NONE',  ( -0.3775338486402941007, 2.665439728940100056E-18, 0.1233678446911569832 ) ) ;
#695 = DIRECTION ( 'NONE',  ( -0.4999999999999760192, 0.000000000000000000, 0.8660254037844524744 ) ) ;
#696 = CARTESIAN_POINT ( 'NONE',  ( -0.2206173157302028232, 4.321611111111110404, -0.2206173157302028232 ) ) ;
#697 = AXIS2_PLACEMENT_3D ( 'NONE', #16054, #6536, #19464 ) ;
#698 = CARTESIAN_POINT ( 'NONE',  ( -0.2206173157302027676, 5.120222222373953969, 0.2206173157302028787 ) ) ;
#699 = EDGE_LOOP ( 'NONE', ( #23726, #16988, #20171, #18010 ) ) ;
#700 = B_SPLINE_CURVE_WITH_KNOTS ( 'NONE', 3,
 ( #1333, #5472, #3158, #14757, #22052, #8763, #3400, #16215, #7069, #14507, #7187, #23627 ),
 .UNSPECIFIED., .F., .F.,
 ( 4, 2, 2, 2, 2, 4 ),
 ( 0.000000000000000000, 0.001386135995484534143, 0.002079203993226801106, 0.002772271990969068286, 0.004158407986453602212, 0.005544543981938136572 ),
 .UNSPECIFIED. ) ;
#701 = CARTESIAN_POINT ( 'NONE',  ( 0.1608054620978590921, 4.576414215844414990, 0.2688593698499974205 ) ) ;
#702 = ORIENTED_EDGE ( 'NONE', *, *, #20635, .F. ) ;
#703 = CARTESIAN_POINT ( 'NONE',  ( 0.4500000000000003442, 0.2598076211353319009, 0.3779506566538943235 ) ) ;
#704 = UNCERTAINTY_MEASURE_WITH_UNIT (LENGTH_MEASURE( 1.000000000000000082E-05 ), #17589, 'distance_accuracy_value', 'NONE');
#705 = CARTESIAN_POINT ( 'NONE',  ( -3.990790521751304672E-07, 4.654944455680286808, -0.3119999999997447038 ) ) ;
#706 = CARTESIAN_POINT ( 'NONE',  ( -3.385114897866767815E-17, -0.2764156081756484196, 0.3800000000000042233 ) ) ;
#707 = CIRCLE ( 'NONE', #14345, 0.3150000000000000022 ) ;
#708 = CARTESIAN_POINT ( 'NONE',  ( 0.08172490057555677201, 4.319272503786364403, -0.3038674704060840281 ) ) ;
#709 = ORIENTED_EDGE ( 'NONE', *, *, #14837, .F. ) ;
#710 = CARTESIAN_POINT ( 'NONE',  ( 0.3613381517857143232, 0.4401785713310289450, 0.000000000000000000 ) ) ;
#711 = CARTESIAN_POINT ( 'NONE',  ( -5.178964085587577574E-17, 0.4104166665908000056, 0.2819296736111110979 ) ) ;
#712 = FACE_OUTER_BOUND ( 'NONE', #6881, .T. ) ;
#713 = DIRECTION ( 'NONE',  ( 1.707404996040164512E-16, 0.000000000000000000, -1.000000000000000000 ) ) ;
#714 = FACE_OUTER_BOUND ( 'NONE', #18143, .T. ) ;
#715 = CARTESIAN_POINT ( 'NONE',  ( 0.2764156081756484196, -5.077672346800151106E-17, 0.2897222222222257115 ) ) ;
#716 = ORIENTED_EDGE ( 'NONE', *, *, #14992, .F. ) ;
#717 = DIRECTION ( 'NONE',  ( -0.000000000000000000, 0.000000000000000000, 1.000000000000000000 ) ) ;
#718 = CARTESIAN_POINT ( 'NONE',  ( 0.01294618724694471777, 0.5474118055169124863, 0.04270874187135767497 ) ) ;
#719 = CARTESIAN_POINT ( 'NONE',  ( -0.3236067977499789694, -1.707404996040164512E-17, -0.2351141009169893104 ) ) ;
#720 = CARTESIAN_POINT ( 'NONE',  ( 0.3119999999999998885, 0.2368055555555552416, 0.1292346314604058410 ) ) ;
#721 = CARTESIAN_POINT ( 'NONE',  ( -0.3119999999999998885, 4.943138888888888083, 0.1292346314604058410 ) ) ;
#722 = CARTESIAN_POINT ( 'NONE',  ( 5.178964085587577574E-17, 3.880638888964754951, 0.2819296736111110979 ) ) ;
#723 = PLANE ( 'NONE',  #3425 ) ;
#724 = CARTESIAN_POINT ( 'NONE',  ( -0.3118573088780928759, 0.3612149761357835165, 0.4243809486557250099 ) ) ;
#725 = CARTESIAN_POINT ( 'NONE',  ( 0.3109237511666488318, 4.807014546080258910, 0.02589370761429525894 ) ) ;
#726 =( BOUNDED_CURVE ( )  B_SPLINE_CURVE ( 2, ( #21271, #14984, #20582, #13399, #3879, #22405, #13842, #217, #15222 ),
 .UNSPECIFIED., .F., .F. ) 
 B_SPLINE_CURVE_WITH_KNOTS ( ( 3, 2, 2, 2, 3 ),
 ( 0.4791666666666666852, 0.4895833333333333148, 0.5000000000000000000, 0.5104166666666666297, 0.5208333333333333703 ),
 .UNSPECIFIED. ) 
 CURVE ( )  GEOMETRIC_REPRESENTATION_ITEM ( )  RATIONAL_B_SPLINE_CURVE ( ( 1.000000000000000000, 0.9238795325112867385, 1.000000000000000000, 0.9238795325112867385, 1.000000000000000000, 0.9238795325112867385, 1.000000000000000000, 0.9238795325112867385, 1.000000000000000000 ) ) 
 REPRESENTATION_ITEM ( '' )  );
#727 = ORIENTED_EDGE ( 'NONE', *, *, #16674, .T. ) ;
#728 = AXIS2_PLACEMENT_3D ( 'NONE', #16579, #7312, #21932 ) ;
#729 = DIRECTION ( 'NONE',  ( 0.8660254037844383745, -3.466132199608281475E-18, 0.5000000000000004441 ) ) ;
#730 = CARTESIAN_POINT ( 'NONE',  ( -0.2819296736111110424, 4.793833333409199149, -0.1167790944451423119 ) ) ;
#731 = CARTESIAN_POINT ( 'NONE',  ( -6.979263641208234666E-17, 0.3330357141881718497, 0.3799334167787516980 ) ) ;
#732 = FACE_OUTER_BOUND ( 'NONE', #19787, .T. ) ;
#733 = COORDINATED_UNIVERSAL_TIME_OFFSET ( 0, 0, .AHEAD. ) ;
#734 = CARTESIAN_POINT ( 'NONE',  ( -0.4687500000000003331, -0.2570931668155775340, 0.04874733047933996893 ) ) ;
#735 = CARTESIAN_POINT ( 'NONE',  ( 0.2206173157302028232, 0.6291666665149338034, -0.2206173157302028232 ) ) ;
#736 = DIMENSIONAL_EXPONENTS ( 1.000000000000000000, 0.000000000000000000, 0.000000000000000000, 0.000000000000000000, 0.000000000000000000, 0.000000000000000000, 0.000000000000000000 ) ;
#737 = CARTESIAN_POINT ( 'NONE',  ( 5.178964085587577574E-17, 4.269527777853643791, 0.2819296736111110979 ) ) ;
#738 = CARTESIAN_POINT ( 'NONE',  ( -0.1962930875501540939, 4.049869897624702730, -0.2425499489820887034 ) ) ;
#739 = CARTESIAN_POINT ( 'NONE',  ( -0.1144950937579609779, 0.2764156081756484196, -0.02624999999999906228 ) ) ;
#740 = CARTESIAN_POINT ( 'NONE',  ( 0.000000000000000000, 2.689999999999999947, -0.8847213396323272416 ) ) ;
#741 = AXIS2_PLACEMENT_3D ( 'NONE', #23126, #21197, #4488 ) ;
#742 = CARTESIAN_POINT ( 'NONE',  ( 0.1167790944451423535, 0.4833333332574667462, 0.2819296736111110424 ) ) ;
#743 = CARTESIAN_POINT ( 'NONE',  ( 0.000000000000000000, 6.000000000000000888, -0.2500000000000000000 ) ) ;
#744 = CARTESIAN_POINT ( 'NONE',  ( 0.1292346314604105595, 4.477861111111109516, -0.3119999999999950591 ) ) ;
#745 = CARTESIAN_POINT ( 'NONE',  ( -0.1236067977499789583, 0.3499999999999998668, -0.3804226065180614791 ) ) ;
#746 = CARTESIAN_POINT ( 'NONE',  ( 0.1306872919485614071, -0.3155070326520293955, 0.2463194444444473108 ) ) ;
#747 = DIRECTION ( 'NONE',  ( -0.000000000000000000, -1.000000000000000000, -0.000000000000000000 ) ) ;
#748 = PLANE ( 'NONE',  #12096 ) ;
#749 = CARTESIAN_POINT ( 'NONE',  ( -0.1993543840281267465, 0.4590277777019111105, 0.1993543840281266633 ) ) ;
#750 = CARTESIAN_POINT ( 'NONE',  ( -0.1993543840281266633, 0.2784722221463555858, -0.1993543840281266910 ) ) ;
#751 = CARTESIAN_POINT ( 'NONE',  ( 0.1167790944451422702, 3.960500000075866556, -0.2819296736111110424 ) ) ;
#752 = CARTESIAN_POINT ( 'NONE',  ( -0.4000000000000000222, 0.2124999998049151573, -4.898587196589413075E-17 ) ) ;
#753 = CARTESIAN_POINT ( 'NONE',  ( 0.1167790944451424368, 4.550777777853644679, 0.2819296736111110424 ) ) ;
#754 = CARTESIAN_POINT ( 'NONE',  ( 1.910449006669871087E-17, 0.1361111109593781676, -0.3119999999999999996 ) ) ;
#755 = ORIENTED_EDGE ( 'NONE', *, *, #13785, .F. ) ;
#756 = CARTESIAN_POINT ( 'NONE',  ( 0.3125000000000000000, -5.740531871003217465E-17, 0.2550000000000030020 ) ) ;
#757 = CARTESIAN_POINT ( 'NONE',  ( 0.3119999999999999996, 3.859805555707287450, 0.1292346314604056190 ) ) ;
#758 = CC_DESIGN_PERSON_AND_ORGANIZATION_ASSIGNMENT ( #6458, #2797, ( #23325 ) ) ;
#759 = CARTESIAN_POINT ( 'NONE',  ( -0.2722827744214833534, 0.3840633442573329615, 0.4172182224143142215 ) ) ;
#760 = VECTOR ( 'NONE', #8554, 39.37007874015748854 ) ;
#761 = LENGTH_MEASURE_WITH_UNIT ( LENGTH_MEASURE( 0.02539999999999999897 ), #1124 );
#762 = DIRECTION ( 'NONE',  ( -0.000000000000000000, -1.000000000000000000, -0.000000000000000000 ) ) ;
#763 = CALENDAR_DATE ( 2026, 7, 10 ) ;
#764 = ORIENTED_EDGE ( 'NONE', *, *, #8568, .T. ) ;
#765 = CARTESIAN_POINT ( 'NONE',  ( 0.2663171304906554182, 0.09313777201924491878, 0.3936412650000162827 ) ) ;
#766 = CARTESIAN_POINT ( 'NONE',  ( -0.2338183013878962213, 5.008588309138786165, 0.2066192498384957776 ) ) ;
#767 = ORIENTED_EDGE ( 'NONE', *, *, #8582, .F. ) ;
#768 = CARTESIAN_POINT ( 'NONE',  ( -0.1993543840281266633, 0.1812499999241333482, -0.1993543840281266910 ) ) ;
#769 = VERTEX_POINT ( 'NONE', #23119 ) ;
#770 = CARTESIAN_POINT ( 'NONE',  ( 0.2842112554124473500, 4.255934241376375660, -0.1287169935595789960 ) ) ;
#771 = DIRECTION ( 'NONE',  ( -0.000000000000000000, -1.000000000000000000, -0.000000000000000000 ) ) ;
#772 = CARTESIAN_POINT ( 'NONE',  ( 7.699581739047377146E-15, 4.099388889040679551, -0.3119999999999999996 ) ) ;
#773 = CARTESIAN_POINT ( 'NONE',  ( 0.2233192592356399997, 0.3616071427596004861, -0.3073725909049500049 ) ) ;
#774 = CARTESIAN_POINT ( 'NONE',  ( 0.1938699776224440674, 5.185072709559078064, -0.2174650966580584655 ) ) ;
#775 = VECTOR ( 'NONE', #528, 39.37007874015748143 ) ;
#776 = EDGE_CURVE ( 'NONE', #12827, #14874, #23357, .T. ) ;
#777 = CARTESIAN_POINT ( 'NONE',  ( 0.2233192592356399164, 0.4294642856167432687, 0.3073725909049500604 ) ) ;
#778 = AXIS2_PLACEMENT_3D ( 'NONE', #4712, #11939, #2766 ) ;
#779 = CARTESIAN_POINT ( 'NONE',  ( -0.2472135954999579444, 0.1303571426620580564, -0.3402603233408160732 ) ) ;
#780 = CARTESIAN_POINT ( 'NONE',  ( -0.1167790944451423535, 4.085500000075865223, 0.2819296736111110424 ) ) ;
#781 = CARTESIAN_POINT ( 'NONE',  ( -0.2206173157302028787, 0.1013888887371559577, 0.2206173157302027954 ) ) ;
#782 = CARTESIAN_POINT ( 'NONE',  ( -0.1792825390751967840, 5.189912767811706296, 0.2278189856582707729 ) ) ;
#783 = DIRECTION ( 'NONE',  ( 0.000000000000000000, 0.000000000000000000, 1.000000000000000000 ) ) ;
#784 = CARTESIAN_POINT ( 'NONE',  ( 0.3119999999999999996, 4.526472222373955745, 0.1292346314604056190 ) ) ;
#785 = ADVANCED_FACE ( 'NONE', ( #4602 ), #584, .T. ) ;
#786 = CARTESIAN_POINT ( 'NONE',  ( 0.1167790944451422702, 4.904944444520310753, -0.2819296736111110979 ) ) ;
#787 = VERTEX_POINT ( 'NONE', #705 ) ;
#788 = CARTESIAN_POINT ( 'NONE',  ( 0.1167790944451424368, 4.092444444520309865, 0.2819296736111110424 ) ) ;
#789 = VERTEX_POINT ( 'NONE', #11944 ) ;
#790 = EDGE_LOOP ( 'NONE', ( #12525, #8590 ) ) ;
#791 = CONICAL_SURFACE ( 'NONE', #3127, 0.3308333333333332571, 0.7853981633974427279 ) ;
#792 = VECTOR ( 'NONE', #15978, 39.37007874015748854 ) ;
#793 = ORIENTED_EDGE ( 'NONE', *, *, #11721, .F. ) ;
#794 = COORDINATED_UNIVERSAL_TIME_OFFSET ( 0, 0, .AHEAD. ) ;
#795 = VERTEX_POINT ( 'NONE', #19475 ) ;
#796 = CARTESIAN_POINT ( 'NONE',  ( 0.1294417382415924134, 0.3124999999999999445, 0.05013888888889062728 ) ) ;
#797 = CARTESIAN_POINT ( 'NONE',  ( 0.1294417382415924134, 0.3124999999999999445, 0.2654166666666697427 ) ) ;
#798 = CARTESIAN_POINT ( 'NONE',  ( -0.3119999999999999996, 0.03541666651493374784, -0.1292346314604056745 ) ) ;
#799 = LINE ( 'NONE', #7545, #21796 ) ;
#800 = LINE ( 'NONE', #23333, #4506 ) ;
#801 = CARTESIAN_POINT ( 'NONE',  ( -0.4687500000000004441, -0.1747720533650699848, 0.4002708887178494379 ) ) ;
#802 = CARTESIAN_POINT ( 'NONE',  ( -0.3119999999999999996, 4.936194444444443441, -0.1292346314604056468 ) ) ;
#803 = FACE_OUTER_BOUND ( 'NONE', #402, .T. ) ;
#804 = CARTESIAN_POINT ( 'NONE',  ( 0.1167790944451423119, 0.6152777777019110550, -0.2819296736111110979 ) ) ;
#805 = CARTESIAN_POINT ( 'NONE',  ( -3.385114897866767815E-17, -0.2764156081756484196, 0.1577777777777801815 ) ) ;
#806 = ORIENTED_EDGE ( 'NONE', *, *, #16313, .F. ) ;
#807 = CARTESIAN_POINT ( 'NONE',  ( 1.726321361862525858E-17, 0.6187499999241333759, -0.2819296736111110979 ) ) ;
#808 = CARTESIAN_POINT ( 'NONE',  ( -0.1993543840281266910, 4.679250000075866112, -0.1993543840281266910 ) ) ;
#809 = DIRECTION ( 'NONE',  ( -0.000000000000000000, -1.000000000000000000, -0.000000000000000000 ) ) ;
#810 = VECTOR ( 'NONE', #17058, 39.37007874015748143 ) ;
#811 = CARTESIAN_POINT ( 'NONE',  ( -0.2501893453879348028, 0.6631137783794425200, -1.085133476862891522 ) ) ;
#812 = DIRECTION ( 'NONE',  ( -1.000000000000000000, 0.000000000000000000, 0.000000000000000000 ) ) ;
#813 = CARTESIAN_POINT ( 'NONE',  ( -1.493307031895086562E-17, 0.4842666352810564567, -1.161472000792705517 ) ) ;
#814 = CARTESIAN_POINT ( 'NONE',  ( 0.3119999999999999996, 4.359805555555555046, -0.1292346314604056745 ) ) ;
#815 = VECTOR ( 'NONE', #18919, 39.37007874015748143 ) ;
#816 = CARTESIAN_POINT ( 'NONE',  ( 0.3119999999999999996, 5.082027777929511103, 0.1292346314604056190 ) ) ;
#817 = ADVANCED_FACE ( 'NONE', ( #13763 ), #15213, .F. ) ;
#818 = CARTESIAN_POINT ( 'NONE',  ( 0.3108786273261404665, 4.973666332255019640, 0.02642876375196673636 ) ) ;
#819 = ORIENTED_EDGE ( 'NONE', *, *, #2364, .F. ) ;
#820 = CARTESIAN_POINT ( 'NONE',  ( 0.2556444780738587608, 4.580106500439447892, 0.1804377530121719919 ) ) ;
#821 = ORIENTED_EDGE ( 'NONE', *, *, #7465, .T. ) ;
#822 = CARTESIAN_POINT ( 'NONE',  ( 5.022068824175014099E-06, 4.710499865219635929, -0.3120000000021129760 ) ) ;
#823 = CARTESIAN_POINT ( 'NONE',  ( 0.1907856466924852668, 4.133017441549366566, 0.2468700812986916737 ) ) ;
#824 = ADVANCED_FACE ( 'NONE', ( #40 ), #14572, .T. ) ;
#825 = CARTESIAN_POINT ( 'NONE',  ( -3.863846776457871776E-17, -0.3155070326520292845, 0.1352083333333357895 ) ) ;
#826 = AXIS2_PLACEMENT_3D ( 'NONE', #7138, #23693, #20181 ) ;
#827 = CARTESIAN_POINT ( 'NONE',  ( -0.1963876315374235015, -0.4278814254316300469, 0.09139303015897908000 ) ) ;
#828 = EDGE_CURVE ( 'NONE', #4354, #12796, #17702, .T. ) ;
#829 = CARTESIAN_POINT ( 'NONE',  ( -0.3613381517857143232, -0.04196428581182810175, -4.425116109941954795E-17 ) ) ;
#830 = EDGE_CURVE ( 'NONE', #2961, #10685, #3831, .T. ) ;
#831 = CARTESIAN_POINT ( 'NONE',  ( 0.1167790944451423119, 0.05972222214635558579, -0.2819296736111110979 ) ) ;
#832 = CARTESIAN_POINT ( 'NONE',  ( 4.113055369932088708E-16, 0.09642857142857140518, 0.4000000000000000222 ) ) ;
#833 = CARTESIAN_POINT ( 'NONE',  ( 0.000000000000000000, 3.738758431839877614E-19, -0.1012499999999999928 ) ) ;
#834 = CARTESIAN_POINT ( 'NONE',  ( -0.1975560007913283733, -0.2122688852238888424, -0.07862277518649050945 ) ) ;
#835 = CARTESIAN_POINT ( 'NONE',  ( 0.000000000000000000, 0.2764156081756484196, 0.4702777777777826795 ) ) ;
#836 = ORIENTED_EDGE ( 'NONE', *, *, #1140, .F. ) ;
#837 = CARTESIAN_POINT ( 'NONE',  ( 0.3950000000000000733, 0.000000000000000000, -0.4000000000000000222 ) ) ;
#838 = CARTESIAN_POINT ( 'NONE',  ( 0.000000000000000000, 3.738758431839877614E-19, 0.4425000000000000044 ) ) ;
#839 = CARTESIAN_POINT ( 'NONE',  ( 0.2078702321837838651, 1.046010598739760082E-17, -0.3061389487775396656 ) ) ;
#840 = CARTESIAN_POINT ( 'NONE',  ( 0.1292346314604057023, 0.5631944444444441089, 0.3119999999999998885 ) ) ;
#841 = CARTESIAN_POINT ( 'NONE',  ( 0.1292346314604056190, 4.977861111111110404, -0.3119999999999999996 ) ) ;
#842 = CARTESIAN_POINT ( 'NONE',  ( -0.2819296736111110424, 4.092444444520309865, 0.1167790944451424923 ) ) ;
#843 = EDGE_CURVE ( 'NONE', #4460, #20446, #15558, .T. ) ;
#844 = DIRECTION ( 'NONE',  ( 1.000000000000000000, -1.821231995776178240E-15, 0.000000000000000000 ) ) ;
#845 = CARTESIAN_POINT ( 'NONE',  ( -1.975393552757948877E-16, 0.5289902422706634910, 0.3941886329748526263 ) ) ;
#846 = CARTESIAN_POINT ( 'NONE',  ( 0.2630554106833125072, -9.196729208309143084E-18, 0.2488419919605451280 ) ) ;
#847 = EDGE_LOOP ( 'NONE', ( #20067, #11056, #922, #8581 ) ) ;
#848 = VERTEX_POINT ( 'NONE', #8395 ) ;
#849 = CARTESIAN_POINT ( 'NONE',  ( -0.3125000000000000000, 1.913510623667739771E-17, 0.1230555555555578606 ) ) ;
#850 = CARTESIAN_POINT ( 'NONE',  ( -0.1993543840281266910, 4.734805555631420582, -0.1993543840281266910 ) ) ;
#851 = CARTESIAN_POINT ( 'NONE',  ( 0.2977100099089716734, 3.575000000000000622, 0.09499999999999993172 ) ) ;
#852 = PERSON_AND_ORGANIZATION_ROLE ( 'design_supplier' ) ;
#853 = CARTESIAN_POINT ( 'NONE',  ( -0.4687500000000003886, 0.04414795829722523157, 0.09139193563994604808 ) ) ;
#854 = CARTESIAN_POINT ( 'NONE',  ( -0.2764156081756484196, -0.1144950937579609362, 0.09180555555555744429 ) ) ;
#855 = CARTESIAN_POINT ( 'NONE',  ( 0.1167790944451422702, 4.238277777853643791, -0.2819296736111110979 ) ) ;
#856 = FACE_OUTER_BOUND ( 'NONE', #8804, .T. ) ;
#857 = CARTESIAN_POINT ( 'NONE',  ( 0.4805070082343983473, 0.2560807851245830991, 0.04413116910601658921 ) ) ;
#858 = CARTESIAN_POINT ( 'NONE',  ( -0.1144950937579609779, 0.2764156081756484196, 0.3070833333333368720 ) ) ;
#859 = CARTESIAN_POINT ( 'NONE',  ( 0.1236067977499789028, 0.2428571428571427715, 0.3804226065180614791 ) ) ;
#860 = CARTESIAN_POINT ( 'NONE',  ( 0.1993543840281266910, 0.5006944443685777957, -0.1993543840281266910 ) ) ;
#861 = CARTESIAN_POINT ( 'NONE',  ( 0.000000000000000000, 3.659999999999999698, 0.3125000000000000000 ) ) ;
#862 = CARTESIAN_POINT ( 'NONE',  ( -0.1868639192671614491, 4.559812086079793048, -3.228500364337123951 ) ) ;
#863 = CARTESIAN_POINT ( 'NONE',  ( -0.3125000000000000000, 1.913510623667739771E-17, 0.005000000000001014917 ) ) ;
#864 = CARTESIAN_POINT ( 'NONE',  ( 0.000000000000000000, 0.3155070326520292845, 0.3817361111111151062 ) ) ;
#865 = DIRECTION ( 'NONE',  ( -0.4985709748471500169, -0.07555085810113110201, -0.8635502596144276621 ) ) ;
#866 = CARTESIAN_POINT ( 'NONE',  ( -0.001104081132507200120, 3.766085226183863099, -0.3119983319538429667 ) ) ;
#867 = CARTESIAN_POINT ( 'NONE',  ( -0.1993543840281266633, 0.4451388888130222710, -0.1993543840281266910 ) ) ;
#868 = CARTESIAN_POINT ( 'NONE',  ( 0.1993543840281266355, 0.5284722221463555858, 0.1993543840281267465 ) ) ;
#869 = CARTESIAN_POINT ( 'NONE',  ( -0.2819296736111110424, 4.036888888964754507, 0.1167790944451424923 ) ) ;
#870 = CARTESIAN_POINT ( 'NONE',  ( -0.4000000000000000222, 0.2874999998049151961, 0.1299678784931624920 ) ) ;
#871 = ADVANCED_FACE ( 'NONE', ( #2795 ), #8408, .F. ) ;
#872 = AXIS2_PLACEMENT_3D ( 'NONE', #24104, #22401, #18505 ) ;
#873 = CARTESIAN_POINT ( 'NONE',  ( 0.2819296736111110979, 4.672305555631421470, -3.452642723725051716E-17 ) ) ;
#874 = ADVANCED_FACE ( 'NONE', ( #10250 ), #21693, .F. ) ;
#875 = CARTESIAN_POINT ( 'NONE',  ( 0.04643634559190757544, -0.5144558407376040865, 0.07050986311825921393 ) ) ;
#876 = CARTESIAN_POINT ( 'NONE',  ( 0.3085878716108892972, 5.079831059683014516, -0.04768157464158169490 ) ) ;
#877 = ORIENTED_EDGE ( 'NONE', *, *, #22131, .F. ) ;
#878 = DIRECTION ( 'NONE',  ( -0.7071067811865477948, -0.7071067811865473507, -1.207317650931791104E-16 ) ) ;
#879 = CARTESIAN_POINT ( 'NONE',  ( -0.1292346314604057023, 3.845916666818398610, 0.3119999999999998885 ) ) ;
#880 = DIRECTION ( 'NONE',  ( 0.8635502596144278842, 0.07555085810113110201, 0.4985709748471496838 ) ) ;
#881 = CARTESIAN_POINT ( 'NONE',  ( 0.01440321200433056920, 0.03242967361111057795, 0.2819296736110772916 ) ) ;
#882 = CARTESIAN_POINT ( 'NONE',  ( -7.892860322346445127E-13, 5.206640035683665957, 0.2819296736111106538 ) ) ;
#883 = CALENDAR_DATE ( 2026, 7, 10 ) ;
#884 = VECTOR ( 'NONE', #16865, 39.37007874015748143 ) ;
#885 = CARTESIAN_POINT ( 'NONE',  ( -0.2255988601820826389, 5.107692461630542802, -0.2129516302912839998 ) ) ;
#886 = PLANE ( 'NONE',  #18636 ) ;
#887 = ORIENTED_EDGE ( 'NONE', *, *, #19117, .T. ) ;
#888 = CARTESIAN_POINT ( 'NONE',  ( -5.178964085587577574E-17, 0.1465277777019111383, 0.2819296736111110979 ) ) ;
#889 = ORIENTED_EDGE ( 'NONE', *, *, #5537, .F. ) ;
#890 = CARTESIAN_POINT ( 'NONE',  ( 0.3039227669911347962, 4.254450600140130767, -0.08153721476616594688 ) ) ;
#891 = CARTESIAN_POINT ( 'NONE',  ( -0.2206173157302027954, 0.3166666666666663188, -0.2206173157302028232 ) ) ;
#892 = LINE ( 'NONE', #4427, #411 ) ;
#893 = CARTESIAN_POINT ( 'NONE',  ( -0.2923287055106771337, 0.1794642856167432687, 0.2123892367102619971 ) ) ;
#894 = CARTESIAN_POINT ( 'NONE',  ( 0.2934402123939894302, 5.178655305724935154, 0.01285040835610953142 ) ) ;
#895 = CC_DESIGN_PERSON_AND_ORGANIZATION_ASSIGNMENT ( #14817, #22235, ( #4493 ) ) ;
#896 = CARTESIAN_POINT ( 'NONE',  ( -0.2233192592356399442, 0.3223214284738860624, -0.3073725909049499494 ) ) ;
#897 = CARTESIAN_POINT ( 'NONE',  ( -0.2472135954999579999, 0.1517857140906294644, 0.3402603233408160732 ) ) ;
#898 = CARTESIAN_POINT ( 'NONE',  ( 0.2819296736111110979, 5.224388888964754507, 0.1167790944451422425 ) ) ;
#899 = CARTESIAN_POINT ( 'NONE',  ( -0.2206173157302027954, 0.08749999984826707655, -0.2206173157302028232 ) ) ;
#900 = LINE ( 'NONE', #17372, #14856 ) ;
#901 = CARTESIAN_POINT ( 'NONE',  ( -0.2064834833177447981, 4.787537442838174506, 0.2372672924203171607 ) ) ;
#902 = CARTESIAN_POINT ( 'NONE',  ( 5.731347020009612645E-17, 4.460500000151732536, 0.3119999999999999996 ) ) ;
#903 = VECTOR ( 'NONE', #18861, 39.37007874015748143 ) ;
#904 = CARTESIAN_POINT ( 'NONE',  ( 0.1167790944451422702, 4.682722222298088433, -0.2819296736111110979 ) ) ;
#905 = ORIENTED_EDGE ( 'NONE', *, *, #22479, .F. ) ;
#906 = EDGE_CURVE ( 'NONE', #14487, #19422, #17768, .T. ) ;
#907 = CARTESIAN_POINT ( 'NONE',  ( -0.2819296736111110424, 4.134111111186976828, 0.1167790944451424923 ) ) ;
#908 = EDGE_LOOP ( 'NONE', ( #16306, #2151, #2824, #8426 ) ) ;
#909 = EDGE_LOOP ( 'NONE', ( #6397, #21370, #16740, #1085, #21888 ) ) ;
#910 = ADVANCED_FACE ( 'NONE', ( #20320 ), #9225, .F. ) ;
#911 = PERSON_AND_ORGANIZATION ( #15518, #2538 ) ;
#912 = ORIENTED_EDGE ( 'NONE', *, *, #19552, .F. ) ;
#913 = DIRECTION ( 'NONE',  ( 0.9618236294503443862, 0.08414866388826429400, -0.2604118050257833716 ) ) ;
#914 = CARTESIAN_POINT ( 'NONE',  ( -0.1166234456863465552, 3.066692553488282957, 2.777423565910347225 ) ) ;
#915 = CARTESIAN_POINT ( 'NONE',  ( -0.2206173157302028787, 0.1013888887371559577, 0.2206173157302027954 ) ) ;
#916 = FACE_OUTER_BOUND ( 'NONE', #339, .T. ) ;
#917 = CARTESIAN_POINT ( 'NONE',  ( -0.4592305972001431980, 0.09034966327427822186, 0.4304950168282474232 ) ) ;
#918 = FACE_OUTER_BOUND ( 'NONE', #18485, .T. ) ;
#919 = CYLINDRICAL_SURFACE ( 'NONE', #3731, 0.3119999999999999996 ) ;
#920 = CYLINDRICAL_SURFACE ( 'NONE', #12495, 0.3119999999999999996 ) ;
#921 = CARTESIAN_POINT ( 'NONE',  ( 0.000000000000000000, 0.2764156081756484196, -0.03666666666666578561 ) ) ;
#922 = ORIENTED_EDGE ( 'NONE', *, *, #3016, .F. ) ;
#923 = FACE_OUTER_BOUND ( 'NONE', #13557, .T. ) ;
#924 = CARTESIAN_POINT ( 'NONE',  ( -0.1167790944451423535, 4.529944444520309865, 0.2819296736111110424 ) ) ;
#925 = CYLINDRICAL_SURFACE ( 'NONE', #11464, 0.3119999999999999996 ) ;
#926 = CARTESIAN_POINT ( 'NONE',  ( -1.515315767888941311E-17, 0.1799999999999999933, -1.242999999999999661 ) ) ;
#927 = LINE ( 'NONE', #2761, #14505 ) ;
#928 = CARTESIAN_POINT ( 'NONE',  ( 0.3125000000000000000, -5.740531871003217465E-17, 0.03277777777777902274 ) ) ;
#929 = CARTESIAN_POINT ( 'NONE',  ( 0.1292346314604056190, 4.200083333333332725, -0.3119999999999999996 ) ) ;
#930 = CARTESIAN_POINT ( 'NONE',  ( 0.3109914489913703228, 4.973703627688673912, 0.02508773589508955792 ) ) ;
#931 = LINE ( 'NONE', #3013, #4292 ) ;
#932 = AXIS2_PLACEMENT_3D ( 'NONE', #14008, #4725, #12197 ) ;
#933 = CARTESIAN_POINT ( 'NONE',  ( 0.1311265150379480604, 4.706765840712305859, -0.2838643453171283970 ) ) ;
#934 = APPLICATION_CONTEXT ( 'configuration controlled 3d designs of mechanical parts and assemblies' ) ;
#935 = EDGE_CURVE ( 'NONE', #4205, #15982, #6797, .T. ) ;
#936 = UNCERTAINTY_MEASURE_WITH_UNIT (LENGTH_MEASURE( 1.000000000000000082E-05 ), #21959, 'distance_accuracy_value', 'NONE');
#937 = CARTESIAN_POINT ( 'NONE',  ( 0.2287940570885543812, 4.134455149918617956, 0.2125776350808679938 ) ) ;
#938 = CARTESIAN_POINT ( 'NONE',  ( -0.1306872919485614903, 0.3155070326520293400, 0.05534722222222404620 ) ) ;
#939 = FACE_OUTER_BOUND ( 'NONE', #20791, .T. ) ;
#940 = EDGE_CURVE ( 'NONE', #1752, #2863, #22250, .T. ) ;
#941 = CARTESIAN_POINT ( 'NONE',  ( 0.2233192592356399164, 0.1973214284738861179, 0.3073725909049500604 ) ) ;
#942 = CARTESIAN_POINT ( 'NONE',  ( 0.1993543840281266355, 0.04236111103524448085, 0.1993543840281267465 ) ) ;
#943 = CARTESIAN_POINT ( 'NONE',  ( 0.1144950937579611444, 0.2764156081756483641, 0.1334722222222244348 ) ) ;
#944 = CARTESIAN_POINT ( 'NONE',  ( -0.2209708691207961373, -0.2209708691207961095, 0.4077777777777823465 ) ) ;
#945 = CARTESIAN_POINT ( 'NONE',  ( -0.2353592251390640433, -0.1755526922479207774, -0.08225883004808118293 ) ) ;
#946 = CARTESIAN_POINT ( 'NONE',  ( 0.1144950937579611444, 0.2764156081756483641, 0.3556944444444484210 ) ) ;
#947 = EDGE_LOOP ( 'NONE', ( #11967, #15478, #188, #18609 ) ) ;
#948 = CARTESIAN_POINT ( 'NONE',  ( -0.1492859955951554296, 4.622732444181830047, 0.2739670279635503802 ) ) ;
#949 = CARTESIAN_POINT ( 'NONE',  ( -0.2443338556138178186, 4.273966251018599394, -0.1950947543421605312 ) ) ;
#950 = CARTESIAN_POINT ( 'NONE',  ( 0.2195630361086305937, -0.1679215936616662852, 0.3880822748423153334 ) ) ;
#951 = CARTESIAN_POINT ( 'NONE',  ( -0.2206173157302028787, 0.3861111111111107386, 0.2206173157302027954 ) ) ;
#952 = CARTESIAN_POINT ( 'NONE',  ( -0.2206173157302027676, 4.946611111111110404, 0.2206173157302028787 ) ) ;
#953 = CARTESIAN_POINT ( 'NONE',  ( -0.1167790944451423119, 4.286888888964754507, -0.2819296736111110979 ) ) ;
#954 = CARTESIAN_POINT ( 'NONE',  ( 0.2819296736111110979, 4.057722222298088433, 0.1167790944451422425 ) ) ;
#955 = FACE_OUTER_BOUND ( 'NONE', #1634, .T. ) ;
#956 = CARTESIAN_POINT ( 'NONE',  ( -0.2491691211423121832, 0.3865828334249355458, 0.4343841983240315785 ) ) ;
#957 = DIRECTION ( 'NONE',  ( 0.000000000000000000, 0.000000000000000000, 1.000000000000000000 ) ) ;
#958 = AXIS2_PLACEMENT_3D ( 'NONE', #9522, #18546, #15139 ) ;
#959 = ORIENTED_EDGE ( 'NONE', *, *, #12477, .F. ) ;
#960 = VERTEX_POINT ( 'NONE', #13561 ) ;
#961 = ORIENTED_EDGE ( 'NONE', *, *, #14696, .F. ) ;
#962 = CARTESIAN_POINT ( 'NONE',  ( -0.04084074333279361091, 4.014960638875646914, 0.3119999946968434190 ) ) ;
#963 = CARTESIAN_POINT ( 'NONE',  ( -0.1993543840281266910, 4.790361111186976828, -0.1993543840281266910 ) ) ;
#964 = CARTESIAN_POINT ( 'NONE',  ( 0.2923287055106771337, 0.0008928570453147542749, -0.2123892367102620249 ) ) ;
#965 = CARTESIAN_POINT ( 'NONE',  ( -0.02574519130974469924, 4.515352010847526465, 0.3109365854241030735 ) ) ;
#966 = ADVANCED_FACE ( 'NONE', ( #4385 ), #20199, .F. ) ;
#967 = EDGE_CURVE ( 'NONE', #9981, #22483, #2651, .T. ) ;
#968 = VECTOR ( 'NONE', #17566, 39.37007874015748143 ) ;
#969 = MECHANICAL_CONTEXT ( 'NONE', #934, 'mechanical' ) ;
#970 = CARTESIAN_POINT ( 'NONE',  ( -0.4687500000000003886, -0.2172202243938534394, 0.07046438675350588654 ) ) ;
#971 = CARTESIAN_POINT ( 'NONE',  ( -0.2764156081756484196, 1.692557448933383907E-17, 0.08833333333333522053 ) ) ;
#972 = CARTESIAN_POINT ( 'NONE',  ( 2.986000000000000210, 2.664999999999999591, -2.591000000000000636 ) ) ;
#973 = CARTESIAN_POINT ( 'NONE',  ( 0.1167790944451424506, 3.995222222298087988, 0.2819296736111110424 ) ) ;
#974 = CARTESIAN_POINT ( 'NONE',  ( 0.2209708691207961651, 0.2209708691207959985, -0.07138888888888847428 ) ) ;
#975 = EDGE_CURVE ( 'NONE', #9761, #10294, #8246, .T. ) ;
#976 = CARTESIAN_POINT ( 'NONE',  ( 0.4000000000000000222, 0.3999999999999999112, 0.000000000000000000 ) ) ;
#977 = CARTESIAN_POINT ( 'NONE',  ( 0.1144950937579611444, 0.2764156081756483641, 0.2445833333333364279 ) ) ;
#978 = LOCAL_TIME ( 21, 9, 13.00000000000000000, #2274 ) ;
#979 = CARTESIAN_POINT ( 'NONE',  ( 0.3613381517857143232, 0.08660714275960043618, -0.1174058825155740587 ) ) ;
#980 = CARTESIAN_POINT ( 'NONE',  ( -0.2819296736111110979, 0.1187499999241333620, -3.452642723725051716E-17 ) ) ;
#981 = CARTESIAN_POINT ( 'NONE',  ( -0.04489076912979070993, 0.2868701433674720191, 0.4014144183689973833 ) ) ;
#982 = CARTESIAN_POINT ( 'NONE',  ( 0.4593750000000003664, -0.2760455974562899262, 0.4425000000000000044 ) ) ;
#983 = CARTESIAN_POINT ( 'NONE',  ( 0.1292346314604107538, 4.457027777777777366, 0.3119999999999950036 ) ) ;
#984 = DIRECTION ( 'NONE',  ( 0.000000000000000000, 0.000000000000000000, -1.000000000000000000 ) ) ;
#985 = CARTESIAN_POINT ( 'NONE',  ( 0.1306872919485614071, -0.3155070326520293955, 0.4129861111111153837 ) ) ;
#986 = CARTESIAN_POINT ( 'NONE',  ( 2.911000000000000032, 0.04999999999999919092, 0.000000000000000000 ) ) ;
#987 = CARTESIAN_POINT ( 'NONE',  ( -0.08166736493278629883, 3.791608634910940800, 0.3038790671151373468 ) ) ;
#988 = CARTESIAN_POINT ( 'NONE',  ( -0.1917386267986692094, 3.843661969516976917, 0.2494960182609696486 ) ) ;
#989 = CARTESIAN_POINT ( 'NONE',  ( -0.1167790944451424368, 0.4069444443685779067, 0.2819296736111110424 ) ) ;
#990 = CARTESIAN_POINT ( 'NONE',  ( 0.2819296736111110979, 4.113277777853643791, 0.1167790944451422425 ) ) ;
#991 = CARTESIAN_POINT ( 'NONE',  ( 0.3236067977499789694, 0.4553571426620580120, 0.2351141009169893659 ) ) ;
#992 = CIRCLE ( 'NONE', #6430, 0.3308333333333332571 ) ;
#993 = CARTESIAN_POINT ( 'NONE',  ( 5.178964085587577574E-17, 4.713972222298088433, 0.2819296736111110979 ) ) ;
#994 = DIRECTION ( 'NONE',  ( -0.000000000000000000, -1.000000000000000000, -0.000000000000000000 ) ) ;
#995 = EDGE_CURVE ( 'NONE', #21184, #3065, #22681, .T. ) ;
#996 = CARTESIAN_POINT ( 'NONE',  ( 4.113055369932088708E-16, 0.1589285712334866096, 0.4000000000000000222 ) ) ;
#997 = ORIENTED_EDGE ( 'NONE', *, *, #3467, .T. ) ;
#998 = CARTESIAN_POINT ( 'NONE',  ( 0.1292346314604019553, 4.811194444444444329, -0.3120000000000036633 ) ) ;
#999 = CARTESIAN_POINT ( 'NONE',  ( -1.910449006669871087E-17, 3.877166666818399055, -0.3119999999999999996 ) ) ;
#1000 = FACE_OUTER_BOUND ( 'NONE', #18833, .T. ) ;
#1001 = B_SPLINE_CURVE_WITH_KNOTS ( 'NONE', 3,
 ( #12567, #23506, #8644, #1456, #19987, #23744 ),
 .UNSPECIFIED., .F., .F.,
 ( 4, 2, 4 ),
 ( 0.000000000000000000, 0.0002551367231383059545, 0.0005102734462766119090 ),
 .UNSPECIFIED. ) ;
#1002 =( NAMED_UNIT ( * ) SI_UNIT ( $, .STERADIAN. ) SOLID_ANGLE_UNIT ( ) );
#1003 = CARTESIAN_POINT ( 'NONE',  ( 0.2413337927286317020, 0.03242967361111052244, 0.1464648618589436124 ) ) ;
#1004 = B_SPLINE_CURVE_WITH_KNOTS ( 'NONE', 3,
 ( #1700, #12703, #23874, #24003, #22299, #16701, #7315, #20118, #7194, #5481, #12946, #5596, #13061, #11217, #20479, #18646, #12822, #1939, #9386, #18767, #14639, #16826, #22423, #2062, #22062, #9503, #5356, #13542, #2546, #19014 ),
 .UNSPECIFIED., .F., .F.,
 ( 4, 2, 1, 1, 1, 1, 1, 1, 2, 2, 2, 2, 2, 2, 2, 2, 2, 4 ),
 ( 0.8863390212757288333, 0.8863434829168148621, 0.8863479445579008908, 0.8863568678400728373, 0.8863747144044168413, 0.8864104075331049604, 0.8864817937904809764, 0.8866245663052331194, 0.8869101113347374055, 0.8874812013937460886, 0.8886233815117632329, 0.8909077417477977434, 0.8931921019838321429, 0.8954764622198666535, 0.8977608224559010530, 0.9000451826919354525, 0.9023295429279699631, 0.9046139031640043626 ),
 .UNSPECIFIED. ) ;
#1005 = CARTESIAN_POINT ( 'NONE',  ( -0.1167790944451423535, 4.918833333409199149, 0.2819296736111110979 ) ) ;
#1006 = DATE_TIME_ROLE ( 'creation_date' ) ;
#1007 = ORIENTED_EDGE ( 'NONE', *, *, #22448, .T. ) ;
#1008 = CARTESIAN_POINT ( 'NONE',  ( -0.4687500000000004441, 0.2598076211353315124, 0.06112444011295375262 ) ) ;
#1009 = DIRECTION ( 'NONE',  ( 0.8660254037844434816, 0.000000000000000000, -0.4999999999999913403 ) ) ;
#1010 = ORIENTED_EDGE ( 'NONE', *, *, #1279, .T. ) ;
#1011 = CARTESIAN_POINT ( 'NONE',  ( 0.1993543840281266910, 0.0006944443685778149775, -0.1993543840281266910 ) ) ;
#1012 = ORIENTED_EDGE ( 'NONE', *, *, #3070, .F. ) ;
#1013 = CARTESIAN_POINT ( 'NONE',  ( 0.2819296736111110424, 0.1083333332574667046, -0.1167790944451423119 ) ) ;
#1014 = CARTESIAN_POINT ( 'NONE',  ( -0.2222495215503474397, 4.717448722450788168, -0.2199230339716857219 ) ) ;
#1015 = CARTESIAN_POINT ( 'NONE',  ( -0.5116234456863466562, 0.4427737985694512046, 2.618652241883199228 ) ) ;
#1016 = CARTESIAN_POINT ( 'NONE',  ( -6.979263641208234666E-17, 0.3330357141881717942, 0.3799334167787516425 ) ) ;
#1017 = CARTESIAN_POINT ( 'NONE',  ( -0.1292346314604007618, 4.484805555555555046, -0.3120000000000049400 ) ) ;
#1018 = ORGANIZATION ( 'NAUO-ORG3', 'UNSPECIFIED', 'UNSPECIFIED' ) ;
#1019 = DIRECTION ( 'NONE',  ( 0.5598087876773550908, -0.5598087876773550908, 0.6109240889655765949 ) ) ;
#1020 = CARTESIAN_POINT ( 'NONE',  ( -0.4620259694561524855, -0.2880908832651560281, 0.04413116910601651982 ) ) ;
#1021 = CARTESIAN_POINT ( 'NONE',  ( 0.1993543840281267465, 3.873694444520310309, 0.1993543840281266633 ) ) ;
#1022 = CARTESIAN_POINT ( 'NONE',  ( 0.04846562453573687035, 5.017398224273947882, 0.3082233696503673959 ) ) ;
#1023 = CARTESIAN_POINT ( 'NONE',  ( 0.1353437200857772471, 0.04934356402903733452, 0.2678729552212573695 ) ) ;
#1024 = CARTESIAN_POINT ( 'NONE',  ( -0.2450396070443827401, 4.773971645789902851, -0.1971973324235511971 ) ) ;
#1025 = CARTESIAN_POINT ( 'NONE',  ( 0.1292346314604058410, 4.519527777929509327, 0.3119999999999998885 ) ) ;
#1026 = AXIS2_PLACEMENT_3D ( 'NONE', #11287, #7737, #9571 ) ;
#1027 = CARTESIAN_POINT ( 'NONE',  ( -0.1993543840281266355, 4.818138888964754507, 0.1993543840281267465 ) ) ;
#1028 = ORIENTED_EDGE ( 'NONE', *, *, #8889, .T. ) ;
#1029 = CARTESIAN_POINT ( 'NONE',  ( -0.1993543840281266910, 4.123694444520309865, -0.1993543840281266910 ) ) ;
#1030 = ORIENTED_EDGE ( 'NONE', *, *, #7036, .F. ) ;
#1031 =( BOUNDED_CURVE ( )  B_SPLINE_CURVE ( 2, ( #17601, #8571, #891, #6616, #21494, #10531, #6501, #19665, #8322 ),
 .UNSPECIFIED., .F., .F. ) 
 B_SPLINE_CURVE_WITH_KNOTS ( ( 3, 2, 2, 2, 3 ),
 ( 0.5208333333333333703, 0.5312500000000000000, 0.5416666666666666297, 0.5520833333333333703, 0.5625000000000000000 ),
 .UNSPECIFIED. ) 
 CURVE ( )  GEOMETRIC_REPRESENTATION_ITEM ( )  RATIONAL_B_SPLINE_CURVE ( ( 1.000000000000000000, 0.9238795325112867385, 1.000000000000000000, 0.9238795325112867385, 1.000000000000000000, 0.9238795325112867385, 1.000000000000000000, 0.9238795325112867385, 1.000000000000000000 ) ) 
 REPRESENTATION_ITEM ( '' )  );
#1032 = VERTEX_POINT ( 'NONE', #13470 ) ;
#1033 = SECURITY_CLASSIFICATION ( '', '', #13915 ) ;
#1034 = APPROVAL_STATUS ( 'not_yet_approved' ) ;
#1035 = ORIENTED_EDGE ( 'NONE', *, *, #9456, .F. ) ;
#1036 = EDGE_CURVE ( 'NONE', #11353, #11100, #8248, .T. ) ;
#1037 = CARTESIAN_POINT ( 'NONE',  ( 0.4687499999999988343, 0.2570931668155638783, 0.04874733047934382002 ) ) ;
#1038 = CARTESIAN_POINT ( 'NONE',  ( 0.2206173157302028232, 0.4694444444444441089, -0.2206173157302028232 ) ) ;
#1039 = CARTESIAN_POINT ( 'NONE',  ( 0.4581189881604794123, 0.2644951211353319120, 0.3941886329748525153 ) ) ;
#1040 = AXIS2_PLACEMENT_3D ( 'NONE', #16463, #12823, #22182 ) ;
#1041 = CARTESIAN_POINT ( 'NONE',  ( -0.1246144517033525162, 4.380716919267113596, -0.2867501499782466046 ) ) ;
#1042 = DIRECTION ( 'NONE',  ( 0.000000000000000000, 0.000000000000000000, -1.000000000000000000 ) ) ;
#1043 = CARTESIAN_POINT ( 'NONE',  ( 0.1915162893076086115, 0.2755058174450264463, -0.7251428721360214658 ) ) ;
#1044 = MANIFOLD_SOLID_BREP ( 'Body-Move/Copy1', #3742 ) ;
#1045 = ORIENTED_EDGE ( 'NONE', *, *, #19956, .T. ) ;
#1046 = CARTESIAN_POINT ( 'NONE',  ( -0.1954553509668046640, 0.1954553509668046918, 0.3591666666666706864 ) ) ;
#1047 = CARTESIAN_POINT ( 'NONE',  ( 0.000000000000000000, 3.659999999999999698, 0.000000000000000000 ) ) ;
#1048 = CARTESIAN_POINT ( 'NONE',  ( -0.1144950937579609918, -0.2764156081756484196, 0.04319444444444596465 ) ) ;
#1049 = CARTESIAN_POINT ( 'NONE',  ( 0.000000000000000000, 0.1199999999999999678, 0.000000000000000000 ) ) ;
#1050 = CARTESIAN_POINT ( 'NONE',  ( 0.1993543840281266633, 4.498694444520309865, -0.1993543840281266910 ) ) ;
#1051 = CARTESIAN_POINT ( 'NONE',  ( -3.827021247335479543E-17, -0.3125000000000000000, 0.4077777777777820134 ) ) ;
#1052 = DIRECTION ( 'NONE',  ( 0.000000000000000000, -1.000000000000000000, 0.000000000000000000 ) ) ;
#1053 = PLANE ( 'NONE',  #15689 ) ;
#1054 = PLANE ( 'NONE',  #22884 ) ;
#1055 = CARTESIAN_POINT ( 'NONE',  ( 0.1292346314604056190, 4.311194444444443441, -0.3119999999999999996 ) ) ;
#1056 = CARTESIAN_POINT ( 'NONE',  ( 0.1292346314604058410, 5.130638889040620931, 0.3119999999999998885 ) ) ;
#1057 = CARTESIAN_POINT ( 'NONE',  ( 0.2831239686220249907, 4.970529875428314703, 0.1329317239649490667 ) ) ;
#1058 = VERTEX_POINT ( 'NONE', #17591 ) ;
#1059 = AXIS2_PLACEMENT_3D ( 'NONE', #13640, #21058, #11801 ) ;
#1060 = CARTESIAN_POINT ( 'NONE',  ( 0.2065268859206847996, 4.578017556304259550, 0.2355640099602401283 ) ) ;
#1061 = CARTESIAN_POINT ( 'NONE',  ( -0.2728548680617166600, 4.886493481094341895, -0.1567155967314854681 ) ) ;
#1062 = CARTESIAN_POINT ( 'NONE',  ( 0.2190263280134926160, 4.134062133123920901, 0.2226461969101928007 ) ) ;
#1063 = CARTESIAN_POINT ( 'NONE',  ( 0.3155070326520292290, -0.1306872919485616569, 0.03451388888889055095 ) ) ;
#1064 = CARTESIAN_POINT ( 'NONE',  ( -0.2819296736111110424, 5.238277777853643791, -0.1167790944451423119 ) ) ;
#1065 = CARTESIAN_POINT ( 'NONE',  ( 0.08166541343684949328, 3.819386461530409616, -0.3038794602980067205 ) ) ;
#1066 = VERTEX_POINT ( 'NONE', #16001 ) ;
#1067 = CARTESIAN_POINT ( 'NONE',  ( 0.2923287055106771337, 0.2151785713310289949, -0.2123892367102620249 ) ) ;
#1068 = SPHERICAL_SURFACE ( 'NONE', #9766, 0.01874999999999999931 ) ;
#1069 = CARTESIAN_POINT ( 'NONE',  ( -0.1144950937579609918, -0.2764156081756484196, -0.06097222222222156013 ) ) ;
#1070 = CARTESIAN_POINT ( 'NONE',  ( 0.3125000000000000000, -5.740531871003217465E-17, 0.08833333333333501236 ) ) ;
#1071 = CARTESIAN_POINT ( 'NONE',  ( 0.000000000000000000, 0.2764156081756484196, 0.3591666666666706309 ) ) ;
#1072 = ORIENTED_EDGE ( 'NONE', *, *, #5116, .T. ) ;
#1073 =( BOUNDED_SURFACE ( )  B_SPLINE_SURFACE ( 3, 2, ( 
 ( #7988, #195, #5802 ),
 ( #22385, #22508, #3860 ),
 ( #11303, #7637, #2990 ),
 ( #19206, #8102, #14207 ),
 ( #2514, #2856, #15907 ),
 ( #4575, #1037, #6641 ) ),
 .UNSPECIFIED., .F., .F., .F. ) 
 B_SPLINE_SURFACE_WITH_KNOTS ( ( 4, 2, 4 ),
 ( 3, 3 ),
 ( 0.001402224832186925365, 0.001901366090229829938, 0.002400507348272734511 ),
 ( 0.000000000000000000, 1.000000000000000000 ),
 .UNSPECIFIED. ) 
 GEOMETRIC_REPRESENTATION_ITEM ( )  RATIONAL_B_SPLINE_SURFACE ( (
 ( 1.000000000000000000, 0.8285407536241359283, 1.000000000000000000),
 ( 1.000000000000000000, 0.8382697314792391108, 1.000000000000000000),
 ( 1.000000000000000000, 0.8433836253084343593, 1.000000000000000000),
 ( 1.000000000000000000, 0.8433992480894421107, 1.000000000000000000),
 ( 1.000000000000000000, 0.8382827608170027034, 1.000000000000000000),
 ( 1.000000000000000000, 0.8285407536241046200, 1.000000000000000000) ) ) 
 REPRESENTATION_ITEM ( '' )  SURFACE ( )  );
#1074 = DIRECTION ( 'NONE',  ( -0.000000000000000000, -1.000000000000000000, -0.000000000000000000 ) ) ;
#1075 = CARTESIAN_POINT ( 'NONE',  ( 0.06335377612981468731, 0.09825908148381588825, 0.3999999999999999667 ) ) ;
#1076 = DIRECTION ( 'NONE',  ( 0.000000000000000000, 0.000000000000000000, -1.000000000000000000 ) ) ;
#1077 = CARTESIAN_POINT ( 'NONE',  ( -5.731347020009612645E-17, 0.4486111111111107386, 0.3119999999999999996 ) ) ;
#1078 = CARTESIAN_POINT ( 'NONE',  ( -0.1292346314604057023, 5.005638888888888083, 0.3119999999999998885 ) ) ;
#1079 = CARTESIAN_POINT ( 'NONE',  ( -0.1167790944451423535, 4.252166666742533074, 0.2819296736111110979 ) ) ;
#1080 = CARTESIAN_POINT ( 'NONE',  ( -0.2819296736111110424, 4.029944444520309865, -0.1167790944451423119 ) ) ;
#1081 = CARTESIAN_POINT ( 'NONE',  ( 1.910449006669871087E-17, 0.5805555554038225319, -0.3119999999999999996 ) ) ;
#1082 = MANIFOLD_SOLID_BREP ( 'Thread1', #19696 ) ;
#1083 = CARTESIAN_POINT ( 'NONE',  ( -0.2537239961729407800, 0.3947782598749492999, 0.4289714952839164819 ) ) ;
#1084 = CARTESIAN_POINT ( 'NONE',  ( 0.000000000000000000, 0.9099999999999988098, 0.000000000000000000 ) ) ;
#1085 = ORIENTED_EDGE ( 'NONE', *, *, #14542, .F. ) ;
#1086 = ORIENTED_EDGE ( 'NONE', *, *, #17053, .F. ) ;
#1087 = CARTESIAN_POINT ( 'NONE',  ( -0.3038794811195862922, 4.004552013912318742, 0.08166531675456255301 ) ) ;
#1088 = CARTESIAN_POINT ( 'NONE',  ( -1.726321361862525858E-17, 4.450083333409198261, -0.2819296736111110979 ) ) ;
#1089 = EDGE_CURVE ( 'NONE', #10194, #22245, #14393, .T. ) ;
#1090 = CARTESIAN_POINT ( 'NONE',  ( -0.3103119043768812757, 4.501276256218609717, -0.03246517880612528190 ) ) ;
#1091 = AXIS2_PLACEMENT_3D ( 'NONE', #21137, #18954, #19068 ) ;
#1092 = DIRECTION ( 'NONE',  ( 0.000000000000000000, 1.000000000000000000, 0.000000000000000000 ) ) ;
#1093 = CARTESIAN_POINT ( 'NONE',  ( -0.2764156081756484196, -0.1144950937579609362, 0.03625000000000147549 ) ) ;
#1094 = CARTESIAN_POINT ( 'NONE',  ( 0.6366666666666670471, 2.473333333333333162, -2.782666666666667066 ) ) ;
#1095 = CARTESIAN_POINT ( 'NONE',  ( -0.2819296736111110979, 4.200083333409199149, 0.000000000000000000 ) ) ;
#1096 = CARTESIAN_POINT ( 'NONE',  ( -0.0006228004652524621668, 4.821629233683148108, -0.3119995338756686443 ) ) ;
#1097 = DIRECTION ( 'NONE',  ( 0.000000000000000000, 0.000000000000000000, -1.000000000000000000 ) ) ;
#1098 = CARTESIAN_POINT ( 'NONE',  ( -0.2764156081756484196, 1.692557448933383907E-17, 0.2619444444444476994 ) ) ;
#1099 = CARTESIAN_POINT ( 'NONE',  ( -0.1116596296178199582, 0.1044642856167432993, -0.3436530038418508792 ) ) ;
#1100 = CARTESIAN_POINT ( 'NONE',  ( -0.1167790944451422702, 0.5666666665908001166, -0.2819296736111110424 ) ) ;
#1101 = CARTESIAN_POINT ( 'NONE',  ( 0.4687500000000002776, 0.08780953131551477719, 0.08855729252016260322 ) ) ;
#1102 = CARTESIAN_POINT ( 'NONE',  ( -2.336494862270849996E-07, 3.904935224540334815, 0.3119999999998144258 ) ) ;
#1103 = LINE ( 'NONE', #2696, #792 ) ;
#1104 = CARTESIAN_POINT ( 'NONE',  ( 2.575339694675500462E-17, 0.3464285714285712525, -0.4205848896953069405 ) ) ;
#1105 = CARTESIAN_POINT ( 'NONE',  ( 0.1306872919485616846, 0.3155070326520292290, 0.3782638888888927853 ) ) ;
#1106 = VERTEX_POINT ( 'NONE', #23229 ) ;
#1107 = DIRECTION ( 'NONE',  ( 0.000000000000000000, 0.000000000000000000, -1.000000000000000000 ) ) ;
#1108 = CARTESIAN_POINT ( 'NONE',  ( -0.1571128864003343839, 3.770594504772994071, -0.2726305689577052660 ) ) ;
#1109 = CARTESIAN_POINT ( 'NONE',  ( 1.910449006669871087E-17, 0.3097222222222218435, -0.3119999999999999996 ) ) ;
#1110 = CARTESIAN_POINT ( 'NONE',  ( 0.1993543840281266355, 0.4729166665908000611, 0.1993543840281267465 ) ) ;
#1111 = EDGE_CURVE ( 'NONE', #7699, #14213, #18549, .T. ) ;
#1112 = CARTESIAN_POINT ( 'NONE',  ( 0.1167790944451424368, 4.161888888964755395, 0.2819296736111110424 ) ) ;
#1113 = AXIS2_PLACEMENT_3D ( 'NONE', #6016, #4554, #12016 ) ;
#1114 = CARTESIAN_POINT ( 'NONE',  ( 0.2233192592356399997, -0.04910714295468524698, -0.3073725909049500049 ) ) ;
#1115 = ORIENTED_EDGE ( 'NONE', *, *, #8759, .F. ) ;
#1116 = CARTESIAN_POINT ( 'NONE',  ( -0.2819296736111110424, 4.703555555631421470, 0.1167790944451424923 ) ) ;
#1117 = CARTESIAN_POINT ( 'NONE',  ( 0.3012075971199598134, 5.132458837216917757, -0.05814740050211916755 ) ) ;
#1118 = DIRECTION ( 'NONE',  ( -0.4999999999999911737, 0.000000000000000000, 0.8660254037844437036 ) ) ;
#1119 = ORIENTED_EDGE ( 'NONE', *, *, #3813, .T. ) ;
#1120 = DIRECTION ( 'NONE',  ( 0.000000000000000000, 0.000000000000000000, -1.000000000000000000 ) ) ;
#1121 = CARTESIAN_POINT ( 'NONE',  ( -0.1993543840281266910, 5.234805555631421470, -0.1993543840281266910 ) ) ;
#1122 = ADVANCED_FACE ( 'NONE', ( #8242 ), #12339, .F. ) ;
#1123 = CARTESIAN_POINT ( 'NONE',  ( -0.1956796206285029427, 0.4282901957204844345, 0.4181140142936810578 ) ) ;
#1124 =( LENGTH_UNIT ( ) NAMED_UNIT ( * ) SI_UNIT ( $, .METRE. ) );
#1125 = LINE ( 'NONE', #17800, #18154 ) ;
#1126 = VECTOR ( 'NONE', #2279, 39.37007874015748854 ) ;
#1127 = CARTESIAN_POINT ( 'NONE',  ( -0.1167790944451423535, 4.807722222298087544, 0.2819296736111110979 ) ) ;
#1128 = COORDINATED_UNIVERSAL_TIME_OFFSET ( 0, 0, .AHEAD. ) ;
#1129 = ORIENTED_EDGE ( 'NONE', *, *, #21873, .F. ) ;
#1130 = CARTESIAN_POINT ( 'NONE',  ( -0.02013615247613211728, 5.100645930978458864, -0.3102850255878896735 ) ) ;
#1131 = EDGE_CURVE ( 'NONE', #11997, #14781, #18722, .T. ) ;
#1132 = CARTESIAN_POINT ( 'NONE',  ( -0.03138891603827507343, 4.570755570789335920, 0.3104503094740446723 ) ) ;
#1133 = EDGE_LOOP ( 'NONE', ( #17618, #3765, #23247, #17240, #2720 ) ) ;
#1134 = CARTESIAN_POINT ( 'NONE',  ( 1.726321361862525858E-17, 0.2298611110352444531, -0.2819296736111110979 ) ) ;
#1135 = FACE_OUTER_BOUND ( 'NONE', #23601, .T. ) ;
#1136 = DIRECTION ( 'NONE',  ( 0.000000000000000000, 0.000000000000000000, -1.000000000000000000 ) ) ;
#1137 = CARTESIAN_POINT ( 'NONE',  ( -0.5116234456863466562, 3.514980167629567998, 2.722575290337332365 ) ) ;
#1138 = CARTESIAN_POINT ( 'NONE',  ( -0.3613381517857143232, 0.1723214284738861513, -4.425116109941954795E-17 ) ) ;
#1139 = CARTESIAN_POINT ( 'NONE',  ( -0.2860141851659954160, 5.054083271882030104, -0.1246764997512364026 ) ) ;
#1140 = EDGE_CURVE ( 'NONE', #18221, #8054, #19506, .T. ) ;
#1141 = PLANE ( 'NONE',  #20540 ) ;
#1142 = CARTESIAN_POINT ( 'NONE',  ( -1.726321361862525858E-17, 4.797305555631421470, -0.2819296736111110979 ) ) ;
#1143 = CARTESIAN_POINT ( 'NONE',  ( 2.311159733195646826, 2.661358883302036293, -2.462236895612579968 ) ) ;
#1144 = CARTESIAN_POINT ( 'NONE',  ( -0.2819296736111110424, 3.745222222298088433, 0.1167790944451424923 ) ) ;
#1145 = CARTESIAN_POINT ( 'NONE',  ( -0.04924783737072570278, 0.04405018457464146553, -0.2895592137998864168 ) ) ;
#1146 = CARTESIAN_POINT ( 'NONE',  ( 0.01963288055412146585, 5.016555562292845494, 0.3115338482637666218 ) ) ;
#1147 = CARTESIAN_POINT ( 'NONE',  ( -0.4620259694561523744, -0.2880908832651560281, 0.04413116910601651982 ) ) ;
#1148 = AXIS2_PLACEMENT_3D ( 'NONE', #15804, #6531, #17632 ) ;
#1149 = CARTESIAN_POINT ( 'NONE',  ( -7.000945310522701902E-17, 0.2303571426620580065, 0.3999999999999999667 ) ) ;
#1150 = CARTESIAN_POINT ( 'NONE',  ( -0.2206173157302027676, 4.453555555707287894, 0.2206173157302028787 ) ) ;
#1151 = CARTESIAN_POINT ( 'NONE',  ( -0.1993543840281266910, 4.804250000075865223, -0.1993543840281266910 ) ) ;
#1152 = EDGE_LOOP ( 'NONE', ( #12346, #17673, #18185, #7554 ) ) ;
#1153 = CARTESIAN_POINT ( 'NONE',  ( -0.1167790944451423535, 4.029944444520309865, 0.2819296736111110424 ) ) ;
#1154 = VERTEX_POINT ( 'NONE', #6579 ) ;
#1155 = ORIENTED_EDGE ( 'NONE', *, *, #10547, .T. ) ;
#1156 = ORIENTED_EDGE ( 'NONE', *, *, #22775, .F. ) ;
#1157 = PERSON_AND_ORGANIZATION ( #15518, #2538 ) ;
#1158 = CARTESIAN_POINT ( 'NONE',  ( -1.399103805173478513E-17, 0.4635611116728546865, -1.084197934689580034 ) ) ;
#1159 = CARTESIAN_POINT ( 'NONE',  ( -0.1166234456863465552, 0.9548081934128058723, 2.777423565910347225 ) ) ;
#1160 = ORIENTED_EDGE ( 'NONE', *, *, #11151, .T. ) ;
#1161 = CARTESIAN_POINT ( 'NONE',  ( 0.2206173157302027676, 0.3374999998482670627, 0.2206173157302028787 ) ) ;
#1162 = AXIS2_PLACEMENT_3D ( 'NONE', #6725, #19531, #11999 ) ;
#1163 = DIRECTION ( 'NONE',  ( 0.000000000000000000, 0.000000000000000000, -1.000000000000000000 ) ) ;
#1164 = CARTESIAN_POINT ( 'NONE',  ( 1.910449006669871087E-17, 0.4694444442927115380, -0.3119999999999999996 ) ) ;
#1165 = CARTESIAN_POINT ( 'NONE',  ( -0.3236067977499789694, 0.3571428571428570398, -0.2351141009169893104 ) ) ;
#1166 = ORIENTED_EDGE ( 'NONE', *, *, #22138, .T. ) ;
#1167 = CARTESIAN_POINT ( 'NONE',  ( 0.3119999999999999996, 0.2333333331816004053, 0.000000000000000000 ) ) ;
#1168 = CARTESIAN_POINT ( 'NONE',  ( -0.2819296736111111534, 0.06666666659080003332, 0.1167790944451422563 ) ) ;
#1169 = CARTESIAN_POINT ( 'NONE',  ( -0.2764156081756484196, 1.692557448933383907E-17, 0.03277777777777921009 ) ) ;
#1170 = ORIENTED_EDGE ( 'NONE', *, *, #22862, .T. ) ;
#1171 = CARTESIAN_POINT ( 'NONE',  ( -0.2819296736111110979, 4.519527777853643791, 0.000000000000000000 ) ) ;
#1172 = CARTESIAN_POINT ( 'NONE',  ( -0.3125000000000000000, 1.913510623667739771E-17, 0.3938888888888930628 ) ) ;
#1173 = CARTESIAN_POINT ( 'NONE',  ( -0.1666623126836255520, 0.2230596288034553121, -1.220164406339562913 ) ) ;
#1174 = DIRECTION ( 'NONE',  ( 0.000000000000000000, 0.000000000000000000, -1.000000000000000000 ) ) ;
#1175 = LINE ( 'NONE', #3006, #7710 ) ;
#1176 = CARTESIAN_POINT ( 'NONE',  ( -0.2206173157302028232, 4.154944444444443441, -0.2206173157302028232 ) ) ;
#1177 = EDGE_CURVE ( 'NONE', #9859, #1821, #19623, .T. ) ;
#1178 = CARTESIAN_POINT ( 'NONE',  ( -0.2209708691207961095, 0.2209708691207961373, 0.1647222222222244903 ) ) ;
#1179 = CARTESIAN_POINT ( 'NONE',  ( 0.2474824800886665510, 4.968567478400213844, 0.1919644361720711512 ) ) ;
#1180 =( BOUNDED_CURVE ( )  B_SPLINE_CURVE ( 2, ( #8103, #553, #680, #797, #22868, #6282, #8224, #15675, #6403 ),
 .UNSPECIFIED., .F., .F. ) 
 B_SPLINE_CURVE_WITH_KNOTS ( ( 3, 2, 2, 2, 3 ),
 ( 0.5625000000000001110, 0.5729166666666667407, 0.5833333333333334814, 0.5937500000000001110, 0.6041666666666667407 ),
 .UNSPECIFIED. ) 
 CURVE ( )  GEOMETRIC_REPRESENTATION_ITEM ( )  RATIONAL_B_SPLINE_CURVE ( ( 0.9999999999999992228, 0.9238795325112875156, 1.000000000000000000, 0.9238795325112867385, 1.000000000000000000, 0.9238795325112867385, 1.000000000000000000, 0.9238795325112859613, 1.000000000000000888 ) ) 
 REPRESENTATION_ITEM ( '' )  );
#1181 = VECTOR ( 'NONE', #1052, 39.37007874015748143 ) ;
#1182 = VECTOR ( 'NONE', #18082, 39.37007874015748143 ) ;
#1183 = DIRECTION ( 'NONE',  ( 1.000000000000000000, 0.000000000000000000, -6.148297094540788948E-16 ) ) ;
#1184 = VERTEX_POINT ( 'NONE', #11850 ) ;
#1185 = CARTESIAN_POINT ( 'NONE',  ( -0.007181820806740507948, 4.877369323082827002, -0.3121677187871257364 ) ) ;
#1186 = CARTESIAN_POINT ( 'NONE',  ( 0.000000000000000000, 0.3155070326520292845, 0.1074305555555577912 ) ) ;
#1187 = CARTESIAN_POINT ( 'NONE',  ( -6.979263641208234666E-17, 0.3508928570453145879, 0.3799334167787516425 ) ) ;
#1188 = FACE_OUTER_BOUND ( 'NONE', #12604, .T. ) ;
#1189 = ORIENTED_EDGE ( 'NONE', *, *, #612, .F. ) ;
#1190 = CIRCLE ( 'NONE', #7429, 0.001000000000000037101 ) ;
#1191 = CARTESIAN_POINT ( 'NONE',  ( 0.2923287055106771337, 0.2866071427596004195, -0.2123892367102620249 ) ) ;
#1192 = AXIS2_PLACEMENT_3D ( 'NONE', #1733, #14549, #6863 ) ;
#1193 = CARTESIAN_POINT ( 'NONE',  ( 0.1993543840281266355, 0.09791666659080004720, 0.1993543840281267465 ) ) ;
#1194 = CARTESIAN_POINT ( 'NONE',  ( 0.2764156081756484196, -5.077672346800151106E-17, -0.04361111111111028865 ) ) ;
#1195 = CARTESIAN_POINT ( 'NONE',  ( 1.573500000000000343, 0.5250000000000000222, -0.3524999999999999800 ) ) ;
#1196 = CARTESIAN_POINT ( 'NONE',  ( -0.1167790944451423535, 5.154944444520309865, 0.2819296736111110424 ) ) ;
#1197 = CARTESIAN_POINT ( 'NONE',  ( 0.1144950937579611444, 0.2764156081756483641, 0.4668055555555604141 ) ) ;
#1198 = ORIENTED_EDGE ( 'NONE', *, *, #8725, .F. ) ;
#1199 = CARTESIAN_POINT ( 'NONE',  ( -0.07953501818328695405, 4.601699271391998636, -0.3023590498254824510 ) ) ;
#1200 = APPROVAL ( #1034, 'UNSPECIFIED' ) ;
#1201 = CARTESIAN_POINT ( 'NONE',  ( -0.2310837057929944205, 4.286504077376945610, 0.2125035569942567704 ) ) ;
#1202 = CARTESIAN_POINT ( 'NONE',  ( -0.4593750000000002554, -0.04467892423992274320, 0.4343810118395207143 ) ) ;
#1203 = CARTESIAN_POINT ( 'NONE',  ( -0.3119999999999999996, 0.4902777777777773682, -3.820898013339742174E-17 ) ) ;
#1204 = CARTESIAN_POINT ( 'NONE',  ( 0.1292346314604056190, 4.755638888888888083, -0.3119999999999999996 ) ) ;
#1205 = CARTESIAN_POINT ( 'NONE',  ( 0.1167790944451424506, 4.203555555631420582, 0.2819296736111110424 ) ) ;
#1206 = CARTESIAN_POINT ( 'NONE',  ( 0.2819296736111110979, 4.002166666742532186, 0.1167790944451422425 ) ) ;
#1207 = CARTESIAN_POINT ( 'NONE',  ( -0.3119999999999999996, 0.5944444442927114824, -3.820898013339742174E-17 ) ) ;
#1208 = MANIFOLD_SOLID_BREP ( 'VarFillet1', #244 ) ;
#1209 = CARTESIAN_POINT ( 'NONE',  ( 0.000000000000000000, 0.000000000000000000, 0.000000000000000000 ) ) ;
#1210 = CARTESIAN_POINT ( 'NONE',  ( 4.194415287079685308E-17, 0.02999999999999995379, -0.3425000000000000266 ) ) ;
#1211 = CARTESIAN_POINT ( 'NONE',  ( 0.1167790944451422702, 4.613277777853643791, -0.2819296736111110424 ) ) ;
#1212 = CARTESIAN_POINT ( 'NONE',  ( 0.000000000000000000, 5.579732050807569621, 0.000000000000000000 ) ) ;
#1213 = CARTESIAN_POINT ( 'NONE',  ( -1.910449006669871087E-17, 3.814666666666665762, -0.3119999999999999996 ) ) ;
#1214 = AXIS2_PLACEMENT_3D ( 'NONE', #20619, #3675, #18551 ) ;
#1215 = APPROVAL_STATUS ( 'not_yet_approved' ) ;
#1216 = CYLINDRICAL_SURFACE ( 'NONE', #8821, 0.1874999999999998335 ) ;
#1217 = CARTESIAN_POINT ( 'NONE',  ( 0.2764156081756483641, -0.1144950937579611167, 0.05708333333333497073 ) ) ;
#1218 = CARTESIAN_POINT ( 'NONE',  ( -0.1167790944451423119, 4.134111111186977716, -0.2819296736111110979 ) ) ;
#1219 = CARTESIAN_POINT ( 'NONE',  ( -0.3116075380362458014, 4.835063446295903233, -0.01613731598427003630 ) ) ;
#1220 = CARTESIAN_POINT ( 'NONE',  ( -0.3124999999999989453, -0.1294417382415932460, 0.2862500000000032796 ) ) ;
#1221 =( BOUNDED_CURVE ( )  B_SPLINE_CURVE ( 2, ( #23758, #12458, #4877, #18049, #19876, #6956, #3170, #14398, #1228, #11308, #17934, #10862, #14274, #23517, #18291, #9475, #8902, #6709, #14518, #16346, #5693, #21822, #21582, #14970, #3412, #1345, #8775, #1588, #9024, #21710, #12579, #3867, #14153, #22392, #20121, #12344, #10502, #21940, #20000, #5233, #12706, #5112, #16797, #16908, #8654, #4994, #78, #3287, #16228, #19760, #2036, #3055, #18741, #10741, #16103, #7523, #13156, #20570, #10620, #9843, #559, #15325, #11557, #2520, #13743, #19341, #20689, #15563, #685, #22755, #4337, #20809, #22871, #9718, #5808, #7875, #4221, #7996, #13629, #21168, #4457, #4098, #21047, #18984, #5926, #6046, #19097, #6166, #2284, #11921, #18862, #10087, #2638, #8109, #11788, #203, #13272, #7644, #22985, #15092, #15448, #22515, #17154, #444, #13513, #20928, #2403, #17274, #13386, #11674, #19213, #9962, #17392, #6290, #3980, #11431, #17029, #2164, #9597, #323, #7762, #15206, #22641, #6650, #1046, #16047, #3000, #23100, #17751, #10449, #23219, #15684, #4697, #6528, #8474 ),
 .UNSPECIFIED., .F., .F. ) 
 B_SPLINE_CURVE_WITH_KNOTS ( ( 3, 2, 2, 2, 2, 2, 2, 2, 2, 2, 2, 2, 2, 2, 2, 2, 2, 2, 2, 2, 2, 2, 2, 2, 2, 2, 2, 2, 2, 2, 2, 2, 2, 2, 2, 2, 2, 2, 2, 2, 2, 2, 2, 2, 2, 2, 2, 2, 2, 2, 2, 2, 2, 2, 2, 2, 2, 2, 2, 2, 2, 2, 2, 2, 2, 2, 2, 3 ),
 ( 0.1232176476950136990, 0.1250000000000000000, 0.1354166666666666574, 0.1458333333333333426, 0.1562500000000000000, 0.1666666666666666574, 0.1770833333333333426, 0.1875000000000000000, 0.1979166666666666574, 0.2083333333333333426, 0.2187500000000000000, 0.2291666666666666574, 0.2395833333333333426, 0.2500000000000000000, 0.2604166666666666852, 0.2708333333333333148, 0.2812500000000000000, 0.2916666666666666852, 0.3020833333333333148, 0.3125000000000000000, 0.3229166666666666852, 0.3333333333333333148, 0.3437500000000000000, 0.3541666666666666852, 0.3645833333333333148, 0.3750000000000000000, 0.3854166666666666852, 0.3958333333333333148, 0.4062500000000000000, 0.4166666666666666852, 0.4270833333333333148, 0.4375000000000000000, 0.4479166666666666852, 0.4583333333333333148, 0.4687500000000000000, 0.4791666666666666852, 0.4895833333333333148, 0.5000000000000000000, 0.5104166666666666297, 0.5208333333333333703, 0.5312500000000000000, 0.5416666666666665186, 0.5520833333333333703, 0.5625000000000000000, 0.5729166666666666297, 0.5833333333333333703, 0.5937500000000000000, 0.6041666666666665186, 0.6145833333333333703, 0.6250000000000000000, 0.6354166666666667407, 0.6458333333333334814, 0.6562500000000000000, 0.6666666666666667407, 0.6770833333333334814, 0.6875000000000000000, 0.6979166666666667407, 0.7083333333333334814, 0.7187500000000000000, 0.7291666666666667407, 0.7395833333333334814, 0.7500000000000000000, 0.7604166666666667407, 0.7708333333333334814, 0.7812500000000000000, 0.7916666666666667407, 0.8020833333333334814, 0.8038656856383126215 ),
 .UNSPECIFIED. ) 
 CURVE ( )  GEOMETRIC_REPRESENTATION_ITEM ( )  RATIONAL_B_SPLINE_CURVE ( ( 0.9784078784059425660, 0.9869753448942262253, 1.000000000000000000, 0.9238795325112867385, 1.000000000000000000, 0.9238795325112867385, 1.000000000000000000, 0.9238795325112867385, 1.000000000000000000, 0.9238795325112867385, 1.000000000000000000, 0.9238795325112867385, 1.000000000000000000, 0.9238795325112867385, 1.000000000000000000, 0.9238795325112867385, 1.000000000000000000, 0.9238795325112867385, 1.000000000000000000, 0.9238795325112867385, 1.000000000000000000, 0.9238795325112867385, 1.000000000000000000, 0.9238795325112867385, 1.000000000000000000, 0.9238795325112867385, 1.000000000000000000, 0.9238795325112867385, 1.000000000000000000, 0.9238795325112867385, 1.000000000000000000, 0.9238795325112867385, 1.000000000000000000, 0.9238795325112867385, 1.000000000000000000, 0.9238795325112867385, 1.000000000000000000, 0.9238795325112867385, 1.000000000000000000, 0.9238795325112867385, 1.000000000000000000, 0.9238795325112867385, 1.000000000000000000, 0.9238795325112867385, 1.000000000000000000, 0.9238795325112867385, 1.000000000000000000, 0.9238795325112867385, 1.000000000000000000, 0.9238795325112867385, 1.000000000000000000, 0.9238795325112867385, 1.000000000000000000, 0.9238795325112867385, 1.000000000000000000, 0.9238795325112867385, 1.000000000000000000, 0.9238795325112867385, 1.000000000000000000, 0.9238795325112867385, 1.000000000000000000, 0.9238795325112867385, 1.000000000000000000, 0.9238795325112867385, 1.000000000000000000, 0.9238795325112867385, 1.000000000000000000, 0.9238795325112867385, 1.000000000000000000, 0.9238795325112867385, 1.000000000000000000, 0.9238795325112867385, 1.000000000000000000, 0.9238795325112867385, 1.000000000000000000, 0.9238795325112867385, 1.000000000000000000, 0.9238795325112867385, 1.000000000000000000, 0.9238795325112867385, 1.000000000000000000, 0.9238795325112867385, 1.000000000000000000, 0.9238795325112867385, 1.000000000000000000, 0.9238795325112867385, 1.000000000000000000, 0.9238795325112867385, 1.000000000000000000, 0.9238795325112867385, 1.000000000000000000, 0.9238795325112867385, 1.000000000000000000, 0.9238795325112867385, 1.000000000000000000, 0.9238795325112867385, 1.000000000000000000, 0.9238795325112867385, 1.000000000000000000, 0.9238795325112867385, 1.000000000000000000, 0.9238795325112867385, 1.000000000000000000, 0.9238795325112867385, 1.000000000000000000, 0.9238795325112867385, 1.000000000000000000, 0.9238795325112867385, 1.000000000000000000, 0.9238795325112867385, 1.000000000000000000, 0.9238795325112867385, 1.000000000000000000, 0.9238795325112867385, 1.000000000000000000, 0.9238795325112867385, 1.000000000000000000, 0.9238795325112867385, 1.000000000000000000, 0.9238795325112867385, 1.000000000000000000, 0.9238795325112867385, 1.000000000000000000, 0.9238795325112867385, 1.000000000000000000, 0.9238795325112867385, 1.000000000000000000, 0.9238795325112867385, 1.000000000000000000, 0.9238795325112867385, 1.000000000000000000, 0.9238795325112867385, 1.000000000000000000, 0.9869753448942777396, 0.9784078784060102896 ) ) 
 REPRESENTATION_ITEM ( '' )  );
#1222 = CARTESIAN_POINT ( 'NONE',  ( -0.1144950937579609918, -0.2764156081756484196, 0.2723611111111143845 ) ) ;
#1223 = CARTESIAN_POINT ( 'NONE',  ( -0.1116596296178200276, 0.06160714275960045561, 0.3436530038418508792 ) ) ;
#1224 = CARTESIAN_POINT ( 'NONE',  ( 0.1167790944451423535, 0.02499999992413337591, 0.2819296736111110424 ) ) ;
#1225 = CARTESIAN_POINT ( 'NONE',  ( 0.000000000000000000, 0.3125000000000000000, -0.05749999999999910738 ) ) ;
#1226 = DIRECTION ( 'NONE',  ( 0.000000000000000000, 0.000000000000000000, 1.000000000000000000 ) ) ;
#1227 = DIRECTION ( 'NONE',  ( -0.000000000000000000, -1.000000000000000000, -0.000000000000000000 ) ) ;
#1228 = CARTESIAN_POINT ( 'NONE',  ( 0.1954553509668047195, 0.1954553509668046085, -0.04361111111111028865 ) ) ;
#1229 = CARTESIAN_POINT ( 'NONE',  ( -3.863846776457871776E-17, -0.3155070326520292845, 0.4095138888888931183 ) ) ;
#1230 = EDGE_CURVE ( 'NONE', #22245, #3381, #5918, .T. ) ;
#1231 = ORIENTED_EDGE ( 'NONE', *, *, #14841, .T. ) ;
#1232 = EDGE_LOOP ( 'NONE', ( #23381, #15668, #18294, #13077 ) ) ;
#1233 = DIRECTION ( 'NONE',  ( 6.123233995738605068E-17, -0.8660254037843519992, 0.5000000000001502132 ) ) ;
#1234 = CARTESIAN_POINT ( 'NONE',  ( -0.3038792844419939687, 3.837724674714062090, 0.08166605555175254771 ) ) ;
#1235 = CARTESIAN_POINT ( 'NONE',  ( 0.1167790944451423257, 0.4347222221463555858, -0.2819296736111110424 ) ) ;
#1236 = CARTESIAN_POINT ( 'NONE',  ( -0.2819296736111110424, 3.974388888964754507, -0.1167790944451423119 ) ) ;
#1237 = CARTESIAN_POINT ( 'NONE',  ( -0.4000000000000000222, 0.4303571426620579898, 0.1299678784931624920 ) ) ;
#1238 = CARTESIAN_POINT ( 'NONE',  ( -0.1167790944451423257, 4.578555555631421470, -0.2819296736111110424 ) ) ;
#1239 = CARTESIAN_POINT ( 'NONE',  ( 0.2095071056370220175, 5.124394802682457950, 0.2256314019847080743 ) ) ;
#1240 = CARTESIAN_POINT ( 'NONE',  ( 0.3104426192702163245, 5.079437309436282355, -0.03361595017585427420 ) ) ;
#1241 = VERTEX_POINT ( 'NONE', #23751 ) ;
#1242 = CARTESIAN_POINT ( 'NONE',  ( -0.3125000000000000000, 1.913510623667739771E-17, 0.4008333333333378712 ) ) ;
#1243 = CARTESIAN_POINT ( 'NONE',  ( -0.2819296736111110979, 5.075083333409198261, 0.000000000000000000 ) ) ;
#1244 = CARTESIAN_POINT ( 'NONE',  ( 0.06767679649697184996, 4.208568552395559159, -0.3050095114520465778 ) ) ;
#1245 = ORIENTED_EDGE ( 'NONE', *, *, #16907, .T. ) ;
#1246 = CARTESIAN_POINT ( 'NONE',  ( 0.2819296736111111534, 4.877166666742532186, 0.1167790944451422563 ) ) ;
#1247 = PERSON_AND_ORGANIZATION ( #15518, #2538 ) ;
#1248 = ORIENTED_EDGE ( 'NONE', *, *, #19558, .F. ) ;
#1249 = CARTESIAN_POINT ( 'NONE',  ( -0.2206173157302027954, 0.3097222220704892726, -0.2206173157302028232 ) ) ;
#1250 = CARTESIAN_POINT ( 'NONE',  ( -0.2206173157302027954, 0.1986111109593781676, -0.2206173157302028232 ) ) ;
#1251 = ORIENTED_EDGE ( 'NONE', *, *, #10383, .T. ) ;
#1252 = CARTESIAN_POINT ( 'NONE',  ( -0.1167790944451424368, 0.3652777777019110550, 0.2819296736111110424 ) ) ;
#1253 = EDGE_LOOP ( 'NONE', ( #10356, #5784, #15552, #17852 ) ) ;
#1254 = PLANE ( 'NONE',  #14415 ) ;
#1255 = DIRECTION ( 'NONE',  ( 0.000000000000000000, 0.000000000000000000, -1.000000000000000000 ) ) ;
#1256 = CARTESIAN_POINT ( 'NONE',  ( 0.3016947543841931867, 4.083248925189674416, 0.07952538849869711379 ) ) ;
#1257 = CARTESIAN_POINT ( 'NONE',  ( -0.2472135954999579444, -0.07500000000000002498, -0.3402603233408159622 ) ) ;
#1258 = CARTESIAN_POINT ( 'NONE',  ( 0.000000000000000000, 3.700000000000000622, 0.000000000000000000 ) ) ;
#1259 = EDGE_CURVE ( 'NONE', #1426, #16231, #1475, .T. ) ;
#1260 = CARTESIAN_POINT ( 'NONE',  ( 0.000000000000000000, 0.000000000000000000, 0.000000000000000000 ) ) ;
#1261 = CARTESIAN_POINT ( 'NONE',  ( -0.3125000000000000000, 0.000000000000000000, 1.326383476483184332 ) ) ;
#1262 = CARTESIAN_POINT ( 'NONE',  ( 0.1993543840281266633, 4.790361111186976828, -0.1993543840281266910 ) ) ;
#1263 = ORIENTED_EDGE ( 'NONE', *, *, #11423, .T. ) ;
#1264 = B_SPLINE_CURVE_WITH_KNOTS ( 'NONE', 3,
 ( #2931, #10389, #21230, #4519, #17811, #8535 ),
 .UNSPECIFIED., .F., .F.,
 ( 4, 2, 4 ),
 ( 0.000000000000000000, 0.003274885906227550415, 0.006549771812455102565 ),
 .UNSPECIFIED. ) ;
#1265 = CARTESIAN_POINT ( 'NONE',  ( -0.3949525857693607089, 5.436648244187127775E-19, 0.06334394204733222178 ) ) ;
#1266 = CARTESIAN_POINT ( 'NONE',  ( 0.1167790944451422702, 3.779944444520310309, -0.2819296736111110424 ) ) ;
#1267 = CARTESIAN_POINT ( 'NONE',  ( -0.2818086106116773903, 0.05407526412938527122, 0.1133068594113698230 ) ) ;
#1268 = CARTESIAN_POINT ( 'NONE',  ( 0.04618426000566567408, 5.017331032664509749, 0.3085723143962725290 ) ) ;
#1269 = CARTESIAN_POINT ( 'NONE',  ( 0.1095210610625794029, 0.04736867464127668403, 0.2773152020650166416 ) ) ;
#1270 = DIRECTION ( 'NONE',  ( -0.000000000000000000, 1.000000000000000000, -0.000000000000000000 ) ) ;
#1271 = CARTESIAN_POINT ( 'NONE',  ( 0.3119999999999999996, 4.311194444596176290, -0.1292346314604056745 ) ) ;
#1272 = CARTESIAN_POINT ( 'NONE',  ( -0.1167790944451423119, 4.745222222298088433, -0.2819296736111110979 ) ) ;
#1273 = EDGE_LOOP ( 'NONE', ( #4711, #3490 ) ) ;
#1274 = CARTESIAN_POINT ( 'NONE',  ( 5.178964085587577574E-17, 3.811194444520309865, 0.2819296736111110979 ) ) ;
#1275 = VECTOR ( 'NONE', #8120, 39.37007874015748143 ) ;
#1276 = ORIENTED_EDGE ( 'NONE', *, *, #23443, .F. ) ;
#1277 = EDGE_CURVE ( 'NONE', #16112, #4354, #2064, .T. ) ;
#1278 = EDGE_CURVE ( 'NONE', #5917, #13125, #17965, .T. ) ;
#1279 = EDGE_CURVE ( 'NONE', #14020, #4825, #1031, .T. ) ;
#1280 = DATE_AND_TIME ( #17988, #16185 ) ;
#1281 = CARTESIAN_POINT ( 'NONE',  ( 0.000000000000000000, 5.500232050807569273, 0.000000000000000000 ) ) ;
#1282 = CARTESIAN_POINT ( 'NONE',  ( 0.3247595264191661668, 2.291712385858714729, -0.9871846966950065250 ) ) ;
#1283 = ORIENTED_EDGE ( 'NONE', *, *, #4380, .F. ) ;
#1284 = CARTESIAN_POINT ( 'NONE',  ( -0.1292346314604058410, 0.3826388887371559022, 0.3119999999999998885 ) ) ;
#1285 = CARTESIAN_POINT ( 'NONE',  ( -0.3037470199460711728, 4.393456864127093908, 0.08219764244668044395 ) ) ;
#1286 = CARTESIAN_POINT ( 'NONE',  ( 0.1292346314604057300, 0.1673611109593781676, 0.3119999999999998885 ) ) ;
#1287 = CARTESIAN_POINT ( 'NONE',  ( 0.1943915731514660183, 0.2820215667548245930, -0.7243746963180275333 ) ) ;
#1288 = EDGE_CURVE ( 'NONE', #18221, #10945, #12489, .T. ) ;
#1289 = ORIENTED_EDGE ( 'NONE', *, *, #20498, .F. ) ;
#1290 = FACE_OUTER_BOUND ( 'NONE', #16990, .T. ) ;
#1291 = CARTESIAN_POINT ( 'NONE',  ( 0.2819296736111110424, 0.08749999992413336203, 0.1167790944451424923 ) ) ;
#1292 = CARTESIAN_POINT ( 'NONE',  ( -0.1954553509668046918, -0.1954553509668046640, 0.1508333333333357063 ) ) ;
#1293 = CIRCLE ( 'NONE', #5566, 0.7500000000000001110 ) ;
#1294 = CARTESIAN_POINT ( 'NONE',  ( -0.1993543840281266910, 4.512583333409199149, -0.1993543840281266910 ) ) ;
#1295 = CARTESIAN_POINT ( 'NONE',  ( 0.1294417382415921358, -0.3125000000000002220, 0.4112500000000042788 ) ) ;
#1296 = CARTESIAN_POINT ( 'NONE',  ( 5.731347020009612645E-17, 4.397999999999999687, 0.3119999999999999996 ) ) ;
#1297 = CARTESIAN_POINT ( 'NONE',  ( -0.2206173157302027954, 0.3652777776260448528, -0.2206173157302028232 ) ) ;
#1298 = CARTESIAN_POINT ( 'NONE',  ( 0.1292346314604056190, 4.088972222222221120, -0.3119999999999999996 ) ) ;
#1299 = DIRECTION ( 'NONE',  ( 0.000000000000000000, 0.000000000000000000, 1.000000000000000000 ) ) ;
#1300 = CARTESIAN_POINT ( 'NONE',  ( 0.1292346314604056190, 4.873694444596176290, -0.3119999999999999996 ) ) ;
#1301 = EDGE_CURVE ( 'NONE', #18764, #15529, #10420, .T. ) ;
#1302 = ORIENTED_EDGE ( 'NONE', *, *, #8448, .T. ) ;
#1303 = DIRECTION ( 'NONE',  ( -0.8459207832372989122, 0.4883925919151526629, -0.2142211582677917558 ) ) ;
#1304 = ORIENTED_EDGE ( 'NONE', *, *, #22713, .F. ) ;
#1305 = DIRECTION ( 'NONE',  ( 0.000000000000000000, 0.000000000000000000, 1.000000000000000000 ) ) ;
#1306 = CIRCLE ( 'NONE', #3636, 0.2500000000000000555 ) ;
#1307 = CARTESIAN_POINT ( 'NONE',  ( -0.2230971623002954152, -0.2230971623002953874, 0.07270833333333528992 ) ) ;
#1308 = DIRECTION ( 'NONE',  ( -0.000000000000000000, -0.000000000000000000, -1.000000000000000000 ) ) ;
#1309 = EDGE_CURVE ( 'NONE', #16532, #21451, #8806, .T. ) ;
#1310 = CARTESIAN_POINT ( 'NONE',  ( -0.3119999999999999996, 4.436194444444443441, -0.1292346314604056468 ) ) ;
#1311 = ADVANCED_FACE ( 'NONE', ( #19789 ), #15889, .T. ) ;
#1312 = CARTESIAN_POINT ( 'NONE',  ( 0.2233192592356399164, 0.2687499999024575703, 0.3073725909049500604 ) ) ;
#1313 = CARTESIAN_POINT ( 'NONE',  ( -5.178964085587577574E-17, 0.1465277777019111383, 0.2819296736111110979 ) ) ;
#1314 = CARTESIAN_POINT ( 'NONE',  ( 0.1144950937579611444, 0.2764156081756483641, 0.07791666666666842433 ) ) ;
#1315 = CARTESIAN_POINT ( 'NONE',  ( -0.1993543840281266910, 5.248694444520310753, -0.1993543840281266910 ) ) ;
#1316 = CARTESIAN_POINT ( 'NONE',  ( -0.2764156081756484196, -0.1144950937579609362, 0.3765277777777819579 ) ) ;
#1317 = VERTEX_POINT ( 'NONE', #19910 ) ;
#1318 = CARTESIAN_POINT ( 'NONE',  ( -0.2205053451214862847, 4.606340970039537908, -0.2212367656121000947 ) ) ;
#1319 = CARTESIAN_POINT ( 'NONE',  ( -0.2905792868698985343, 4.276554290496439314, -0.1163786327526087350 ) ) ;
#1320 = CARTESIAN_POINT ( 'NONE',  ( -0.4584510057643288450, -0.2214217964837244257, 0.4064568219641767066 ) ) ;
#1321 = CARTESIAN_POINT ( 'NONE',  ( 0.3119999999999998885, 0.4590277777777774793, 0.1292346314604058410 ) ) ;
#1322 = CARTESIAN_POINT ( 'NONE',  ( -0.3119999999999999996, 4.658416666666666650, -0.1292346314604056468 ) ) ;
#1323 = CARTESIAN_POINT ( 'NONE',  ( 0.1993543840281267465, 3.929250000075865668, 0.1993543840281266633 ) ) ;
#1324 = VECTOR ( 'NONE', #23404, 39.37007874015748854 ) ;
#1325 = CARTESIAN_POINT ( 'NONE',  ( -5.731347020009612645E-17, 0.6083333331816004330, 0.3119999999999999996 ) ) ;
#1326 = FACE_OUTER_BOUND ( 'NONE', #19357, .T. ) ;
#1327 = CARTESIAN_POINT ( 'NONE',  ( 0.000000000000000000, 5.072999999999999510, 0.000000000000000000 ) ) ;
#1328 = ORIENTED_EDGE ( 'NONE', *, *, #16781, .T. ) ;
#1329 = FACE_OUTER_BOUND ( 'NONE', #8390, .T. ) ;
#1330 = CARTESIAN_POINT ( 'NONE',  ( 0.1993543840281267465, 4.595916666742532186, 0.1993543840281266633 ) ) ;
#1331 = CARTESIAN_POINT ( 'NONE',  ( -0.3134171556598066011, 4.502164757452278288, -0.0009694151472935294252 ) ) ;
#1332 = APPROVAL_DATE_TIME ( #15964, #18042 ) ;
#1333 = CARTESIAN_POINT ( 'NONE',  ( -0.03651601414465285855, -0.2739930093161157543, -0.06558227484231510251 ) ) ;
#1334 = CARTESIAN_POINT ( 'NONE',  ( -3.385114897866767815E-17, -0.2764156081756484196, -0.008888888888887782128 ) ) ;
#1335 = CARTESIAN_POINT ( 'NONE',  ( -1.726321361862525858E-17, 4.186194444520309865, -0.2819296736111110979 ) ) ;
#1336 = AXIS2_PLACEMENT_3D ( 'NONE', #7411, #5575, #3751 ) ;
#1337 = CARTESIAN_POINT ( 'NONE',  ( -0.1294417382415922191, 0.3125000000000000000, -0.06097222222222172666 ) ) ;
#1338 = CYLINDRICAL_SURFACE ( 'NONE', #15578, 0.09499999999999995948 ) ;
#1339 = CARTESIAN_POINT ( 'NONE',  ( 0.1144950937579609085, -0.2764156081756484751, 0.2237500000000029188 ) ) ;
#1340 = CARTESIAN_POINT ( 'NONE',  ( 0.3613381517857143232, 0.01160714275960045803, 0.000000000000000000 ) ) ;
#1341 = CARTESIAN_POINT ( 'NONE',  ( 0.1167790944451423535, 0.08055555547968892838, 0.2819296736111110424 ) ) ;
#1342 = CARTESIAN_POINT ( 'NONE',  ( -0.3125000000000000000, 1.913510623667739771E-17, -0.04361111111111011518 ) ) ;
#1343 = CARTESIAN_POINT ( 'NONE',  ( 0.000000000000000000, 0.06786299768266475241, 0.000000000000000000 ) ) ;
#1344 = CARTESIAN_POINT ( 'NONE',  ( -0.02810654887314226191, 0.1573129472011667584, -0.7495061196176546758 ) ) ;
#1345 = CARTESIAN_POINT ( 'NONE',  ( 0.1144950937579611444, 0.2764156081756483641, 0.01541666666666797678 ) ) ;
#1346 = CARTESIAN_POINT ( 'NONE',  ( -0.1306872919485615459, -0.3155070326520293400, 0.3504861111111148286 ) ) ;
#1347 = EDGE_LOOP ( 'NONE', ( #11006, #21584, #11418, #2986 ) ) ;
#1348 = ORIENTED_EDGE ( 'NONE', *, *, #12774, .T. ) ;
#1349 = CARTESIAN_POINT ( 'NONE',  ( 2.986000000000000210, 0.05000000000000028727, -2.541000000000000369 ) ) ;
#1350 = LINE ( 'NONE', #18054, #23745 ) ;
#1351 = CARTESIAN_POINT ( 'NONE',  ( 0.1993543840281266910, 0.4312499999241333759, -0.1993543840281266910 ) ) ;
#1352 = CARTESIAN_POINT ( 'NONE',  ( -0.2819296736111110979, 3.811194444520310309, 0.000000000000000000 ) ) ;
#1353 = CARTESIAN_POINT ( 'NONE',  ( -0.2923287055106771337, 0.04017857133102904071, -0.2123892367102620804 ) ) ;
#1354 = CARTESIAN_POINT ( 'NONE',  ( -0.2819296736111110424, 4.363277777853643791, -0.1167790944451423119 ) ) ;
#1355 = PRODUCT ( '94902A107_High-Strength Steel Flange Nut_94902A107', '94902A107_High-Strength Steel Flange Nut_94902A107', '', ( #21098 ) ) ;
#1356 = CARTESIAN_POINT ( 'NONE',  ( 0.2236628504143657326, 5.124892759571328504, 0.2114858233200252735 ) ) ;
#1357 = EDGE_CURVE ( 'NONE', #11906, #2863, #13132, .T. ) ;
#1358 = CARTESIAN_POINT ( 'NONE',  ( -0.1292346314604058410, 0.1604166665149337478, 0.3119999999999998885 ) ) ;
#1359 = EDGE_LOOP ( 'NONE', ( #877, #5213, #496, #3710, #14056, #447 ) ) ;
#1360 = CARTESIAN_POINT ( 'NONE',  ( 0.1292346314604070623, 4.790361111111110404, 0.3119999999999986673 ) ) ;
#1361 = CARTESIAN_POINT ( 'NONE',  ( 0.2819296736111110424, 5.161888888964753619, -0.1167790944451423396 ) ) ;
#1362 = VECTOR ( 'NONE', #20588, 39.37007874015748143 ) ;
#1363 = CARTESIAN_POINT ( 'NONE',  ( 0.08265232788921492157, 4.208131977080836528, -0.3012013616566489027 ) ) ;
#1364 = CC_DESIGN_PERSON_AND_ORGANIZATION_ASSIGNMENT ( #11727, #7925, ( #19708 ) ) ;
#1365 =( BOUNDED_CURVE ( )  B_SPLINE_CURVE ( 2, ( #10894, #5148, #12614 ),
 .UNSPECIFIED., .F., .T. ) 
 B_SPLINE_CURVE_WITH_KNOTS ( ( 3, 3 ),
 ( 0.8125000000000001110, 0.8163014546100183511 ),
 .UNSPECIFIED. ) 
 CURVE ( )  GEOMETRIC_REPRESENTATION_ITEM ( )  RATIONAL_B_SPLINE_CURVE ( ( 0.9999999999999992228, 0.9722206238030344227, 0.9647168388458877697 ) ) 
 REPRESENTATION_ITEM ( '' )  );
#1366 = LENGTH_MEASURE_WITH_UNIT ( LENGTH_MEASURE( 0.02539999999999999897 ), #16604 );
#1367 =( BOUNDED_CURVE ( )  B_SPLINE_CURVE ( 2, ( #2710, #998, #15874, #17831, #23291, #23415, #8309, #1360, #15760 ),
 .UNSPECIFIED., .F., .F. ) 
 B_SPLINE_CURVE_WITH_KNOTS ( ( 3, 2, 2, 2, 3 ),
 ( 0.2946428571428569843, 0.2991071428571426827, 0.3035714285714284366, 0.3080357142857141906, 0.3124999999999999445 ),
 .UNSPECIFIED. ) 
 CURVE ( )  GEOMETRIC_REPRESENTATION_ITEM ( )  RATIONAL_B_SPLINE_CURVE ( ( 1.000000000000002887, 0.9238795325112838519, 1.000000000000000000, 0.9238795325112867385, 1.000000000000000000, 0.9238795325112867385, 1.000000000000000000, 0.9238795325112877377, 0.9999999999999990008 ) ) 
 REPRESENTATION_ITEM ( '' )  );
#1368 = APPROVAL_PERSON_ORGANIZATION ( #3157, #10165, #3739 ) ;
#1369 = CARTESIAN_POINT ( 'NONE',  ( 0.1167790944451424506, 4.870222222298087544, 0.2819296736111110424 ) ) ;
#1370 = ORIENTED_EDGE ( 'NONE', *, *, #18301, .T. ) ;
#1371 = FACE_OUTER_BOUND ( 'NONE', #3579, .T. ) ;
#1372 = CARTESIAN_POINT ( 'NONE',  ( -0.1292346314604058410, 0.2159722220704893003, 0.3119999999999998885 ) ) ;
#1373 = EDGE_LOOP ( 'NONE', ( #10622, #6711, #23887, #607 ) ) ;
#1374 = CARTESIAN_POINT ( 'NONE',  ( -0.1993543840281266633, 0.3479166665908000056, -0.1993543840281266910 ) ) ;
#1375 = ORIENTED_EDGE ( 'NONE', *, *, #20910, .T. ) ;
#1376 = CARTESIAN_POINT ( 'NONE',  ( -0.1993543840281267465, 0.02847222214635559273, 0.1993543840281266633 ) ) ;
#1377 = LINE ( 'NONE', #18077, #19336 ) ;
#1378 = CARTESIAN_POINT ( 'NONE',  ( -0.4366234456863466451, 0.9548081934128056503, 2.592671479769666387 ) ) ;
#1379 = CARTESIAN_POINT ( 'NONE',  ( -0.4000000000000000222, 0.07857142857142855596, -4.898587196589413075E-17 ) ) ;
#1380 = CARTESIAN_POINT ( 'NONE',  ( -0.2146400242025152671, 5.064908869111506284, 0.2268182928792843722 ) ) ;
#1381 = CARTESIAN_POINT ( 'NONE',  ( 0.8977114317029943891, 2.978485840173427324, -0.6898620042323803103 ) ) ;
#1382 = CARTESIAN_POINT ( 'NONE',  ( 0.1988757138996042617, 3.752970977545328157, -0.2404006040361021113 ) ) ;
#1383 = DIRECTION ( 'NONE',  ( 0.000000000000000000, 0.000000000000000000, -1.000000000000000000 ) ) ;
#1384 = CARTESIAN_POINT ( 'NONE',  ( 0.1167790944451422702, 4.571611111186976828, -0.2819296736111110424 ) ) ;
#1385 = CARTESIAN_POINT ( 'NONE',  ( 0.2608937378291124043, 4.524766547629808677, 0.1723236813421265556 ) ) ;
#1386 = CARTESIAN_POINT ( 'NONE',  ( -0.2819296736111110979, 3.741750000075865668, 0.000000000000000000 ) ) ;
#1387 = CARTESIAN_POINT ( 'NONE',  ( 0.000000000000000000, 2.735000000000000320, 0.000000000000000000 ) ) ;
#1388 = CARTESIAN_POINT ( 'NONE',  ( 0.08162334319253711223, 4.907349590646077786, 0.3038879386963563856 ) ) ;
#1389 = CC_DESIGN_APPROVAL ( #17441, ( #19252 ) ) ;
#1390 = CARTESIAN_POINT ( 'NONE',  ( -0.4687500000000004441, -0.2598076211353211873, 0.06112444011295848495 ) ) ;
#1391 = CARTESIAN_POINT ( 'NONE',  ( -4.638126268221291196E-16, 0.1946428569477723358, -0.4000000000000000222 ) ) ;
#1392 = ADVANCED_FACE ( 'NONE', ( #2964 ), #17845, .T. ) ;
#1393 = CARTESIAN_POINT ( 'NONE',  ( -0.1292346314604057023, 4.401472222373953080, 0.3119999999999998885 ) ) ;
#1394 = CARTESIAN_POINT ( 'NONE',  ( 0.1993543840281266633, 4.679250000075866112, -0.1993543840281266910 ) ) ;
#1395 = CARTESIAN_POINT ( 'NONE',  ( -0.1993543840281266355, 3.915361111186976384, 0.1993543840281267465 ) ) ;
#1396 = ORIENTED_EDGE ( 'NONE', *, *, #15440, .T. ) ;
#1397 = AXIS2_PLACEMENT_3D ( 'NONE', #12766, #12889, #16528 ) ;
#1398 = ADVANCED_FACE ( 'NONE', ( #21379 ), #10296, .F. ) ;
#1399 = EDGE_LOOP ( 'NONE', ( #14770, #23212, #11213, #18691 ) ) ;
#1400 = PERSON_AND_ORGANIZATION_ROLE ( 'creator' ) ;
#1401 = CARTESIAN_POINT ( 'NONE',  ( -0.4749999999999999778, 3.575000000000000622, 0.09499999999999995948 ) ) ;
#1402 = CARTESIAN_POINT ( 'NONE',  ( 0.3124999999999993339, -0.1294417382415928852, 0.2584722222222255450 ) ) ;
#1403 = LOCAL_TIME ( 21, 9, 13.00000000000000000, #14665 ) ;
#1404 = ORIENTED_EDGE ( 'NONE', *, *, #20695, .T. ) ;
#1405 = CARTESIAN_POINT ( 'NONE',  ( -5.731347020009612645E-17, 0.2194444442927115380, 0.3119999999999999996 ) ) ;
#1406 = CARTESIAN_POINT ( 'NONE',  ( -0.0001215146640037667272, 4.377169931752053600, -0.3119999823201240474 ) ) ;
#1407 = CARTESIAN_POINT ( 'NONE',  ( -0.1884418442843545372, 5.123706002978354768, 0.2436494946675597795 ) ) ;
#1408 = DIRECTION ( 'NONE',  ( 0.000000000000000000, 1.000000000000000000, 0.000000000000000000 ) ) ;
#1409 = CARTESIAN_POINT ( 'NONE',  ( -0.3236067977499790249, 0.3714285714285713302, 0.2351141009169892271 ) ) ;
#1410 = ORIENTED_EDGE ( 'NONE', *, *, #9910, .T. ) ;
#1411 = APPLICATION_CONTEXT ( 'configuration controlled 3d designs of mechanical parts and assemblies' ) ;
#1412 = CLOSED_SHELL ( 'NONE', ( #12987, #6790, #364, #17901, #12182, #12813, #20594, #21833, #7393, #5463, #20530, #15707, #668, #3513, #7337, #21407, #21667, #14357, #3608 ) ) ;
#1413 = CARTESIAN_POINT ( 'NONE',  ( 0.2338198238642340554, 5.079091233363342006, 0.2073940069782997664 ) ) ;
#1414 = CARTESIAN_POINT ( 'NONE',  ( -0.1993543840281267465, 0.1812499999241333759, 0.1993543840281266633 ) ) ;
#1415 = CARTESIAN_POINT ( 'NONE',  ( -0.1954553509668046918, -0.1954553509668046640, 0.2063888888888917028 ) ) ;
#1416 = ORIENTED_EDGE ( 'NONE', *, *, #7936, .F. ) ;
#1417 = CARTESIAN_POINT ( 'NONE',  ( 5.178964085587577574E-17, 4.477861111186976828, 0.2819296736111110979 ) ) ;
#1418 = CARTESIAN_POINT ( 'NONE',  ( 0.2816345655934815451, 0.09282869753838597637, -0.08510099145262348119 ) ) ;
#1419 = B_SPLINE_CURVE_WITH_KNOTS ( 'NONE', 3,
 ( #13511, #19339, #801, #556, #8106, #6407, #2752, #17628, #15799, #23218, #21406, #15561 ),
 .UNSPECIFIED., .F., .F.,
 ( 4, 2, 2, 2, 2, 4 ),
 ( 0.000000000000000000, 0.003341087407395306689, 0.005011631111092960250, 0.006682174814790614245, 0.01002326222218592224, 0.01336434962958123196 ),
 .UNSPECIFIED. ) ;
#1420 = CARTESIAN_POINT ( 'NONE',  ( 1.573500000000000343, 2.683750000000000746, -1.818749999999999645 ) ) ;
#1421 = DIRECTION ( 'NONE',  ( -1.493785812010397745E-17, 1.000000000000000000, 0.000000000000000000 ) ) ;
#1422 = CARTESIAN_POINT ( 'NONE',  ( 0.3119999999999999996, 4.137583333333332725, -0.1292346314604056745 ) ) ;
#1423 = EDGE_CURVE ( 'NONE', #15906, #17792, #1377, .T. ) ;
#1424 = CARTESIAN_POINT ( 'NONE',  ( -0.1292346314604057023, 5.012583333485065573, 0.3119999999999998885 ) ) ;
#1425 = CARTESIAN_POINT ( 'NONE',  ( -0.2933322049817026489, 5.157132068594114216, 0.06571910644767618714 ) ) ;
#1426 = VERTEX_POINT ( 'NONE', #6862 ) ;
#1427 = CARTESIAN_POINT ( 'NONE',  ( 5.731347020009612645E-17, 4.175777777777776478, 0.3119999999999999996 ) ) ;
#1428 = EDGE_CURVE ( 'NONE', #4057, #606, #2731, .T. ) ;
#1429 = CARTESIAN_POINT ( 'NONE',  ( -0.09925723254180866817, 4.880039691319455031, -0.2961790094676920448 ) ) ;
#1430 = AXIS2_PLACEMENT_3D ( 'NONE', #14112, #13650, #12062 ) ;
#1431 = CARTESIAN_POINT ( 'NONE',  ( -0.3155070326520293400, -0.1306872919485614626, 0.3470138888888930073 ) ) ;
#1432 = CARTESIAN_POINT ( 'NONE',  ( -0.2923287055106771337, 0.3258928570453146767, -0.2123892367102620804 ) ) ;
#1433 = EDGE_LOOP ( 'NONE', ( #3290, #23860, #7001, #1189 ) ) ;
#1434 = DIRECTION ( 'NONE',  ( -1.000000000000000000, -1.224646799147353700E-16, 0.000000000000000000 ) ) ;
#1435 = CARTESIAN_POINT ( 'NONE',  ( -0.1116596296178200276, 0.1151785713310290032, 0.3436530038418508792 ) ) ;
#1436 = CARTESIAN_POINT ( 'NONE',  ( -0.2819296736111110979, 0.3548611110352444808, -3.452642723725051716E-17 ) ) ;
#1437 = CARTESIAN_POINT ( 'NONE',  ( -0.2764156081756484196, -0.1144950937579609362, 0.09875000000000193345 ) ) ;
#1438 = CARTESIAN_POINT ( 'NONE',  ( 0.2819296736111110979, 5.113277777853642903, 0.1167790944451422425 ) ) ;
#1439 = CARTESIAN_POINT ( 'NONE',  ( -0.4749999999999999778, 3.700000000000000622, 0.09499999999999995948 ) ) ;
#1440 = DIRECTION ( 'NONE',  ( 0.08715574274765829077, -0.9961946980917454342, 0.000000000000000000 ) ) ;
#1441 = LINE ( 'NONE', #6682, #16065 ) ;
#1442 = CARTESIAN_POINT ( 'NONE',  ( 0.2209708691207961651, 0.2209708691207959985, 0.3175000000000035016 ) ) ;
#1443 = CARTESIAN_POINT ( 'NONE',  ( -0.1292346314604056745, 4.762583333333332725, -0.3119999999999999996 ) ) ;
#1444 = VECTOR ( 'NONE', #19758, 39.37007874015748854 ) ;
#1445 = CARTESIAN_POINT ( 'NONE',  ( 5.178964085587577574E-17, 4.088972222298087544, 0.2819296736111110979 ) ) ;
#1446 = CARTESIAN_POINT ( 'NONE',  ( 0.2819296736111110979, 3.779944444520310309, 0.1167790944451422425 ) ) ;
#1447 = CARTESIAN_POINT ( 'NONE',  ( 0.1777386203871747228, 4.021449974115596682, 0.2564743595758844918 ) ) ;
#1448 = MANIFOLD_SOLID_BREP ( 'Thread2', #11535 ) ;
#1449 = DIRECTION ( 'NONE',  ( -0.8660254037844420383, 0.000000000000000000, -0.4999999999999942268 ) ) ;
#1450 = ORIENTED_EDGE ( 'NONE', *, *, #8496, .T. ) ;
#1451 = CARTESIAN_POINT ( 'NONE',  ( 0.000000000000000000, 3.738758431839877614E-19, -0.1016666666666665164 ) ) ;
#1452 = CARTESIAN_POINT ( 'NONE',  ( 5.178964085587577574E-17, 4.477861111186976828, 0.2819296736111110979 ) ) ;
#1453 = EDGE_CURVE ( 'NONE', #11367, #8566, #16136, .T. ) ;
#1454 = CARTESIAN_POINT ( 'NONE',  ( -0.02716817033992858718, 4.489059518347089828, -0.3108624770087871081 ) ) ;
#1455 = COORDINATED_UNIVERSAL_TIME_OFFSET ( 0, 0, .AHEAD. ) ;
#1456 = CARTESIAN_POINT ( 'NONE',  ( -0.4679241437345806331, -0.2662683654317171134, 0.05892738626661206403 ) ) ;
#1457 = CARTESIAN_POINT ( 'NONE',  ( -0.1954553509668046640, 0.1954553509668046918, 0.3036111111111147176 ) ) ;
#1458 = CARTESIAN_POINT ( 'NONE',  ( -0.1167790944451423119, 4.189666666742533074, -0.2819296736111110979 ) ) ;
#1459 = CARTESIAN_POINT ( 'NONE',  ( 0.000000000000000000, 0.3125000000000000000, -0.06444444444444397124 ) ) ;
#1460 = CARTESIAN_POINT ( 'NONE',  ( -0.1166234456863257940, 4.111524471938507119, -2.868834514064774854 ) ) ;
#1461 = CYLINDRICAL_SURFACE ( 'NONE', #22916, 0.4000000000000000222 ) ;
#1462 = CARTESIAN_POINT ( 'NONE',  ( -0.3613381517857144343, -0.02053571438325667298, 0.1174058825155740171 ) ) ;
#1463 = CARTESIAN_POINT ( 'NONE',  ( -0.2819296736111110424, 0.3374999999241334314, -0.1167790944451423396 ) ) ;
#1464 = CARTESIAN_POINT ( 'NONE',  ( 0.3125000000000009437, 0.1294417382415912476, -0.06791666666666591745 ) ) ;
#1465 = CARTESIAN_POINT ( 'NONE',  ( 0.4000000000000000222, 0.03392857123348663045, 0.000000000000000000 ) ) ;
#1466 = CARTESIAN_POINT ( 'NONE',  ( -0.2030836461269783511, 0.4272172410711764790, -0.7219876546682471030 ) ) ;
#1467 = DIRECTION ( 'NONE',  ( 0.000000000000000000, 0.000000000000000000, -1.000000000000000000 ) ) ;
#1468 = CARTESIAN_POINT ( 'NONE',  ( 0.2764156081756484196, -5.077672346800151106E-17, 0.01194444444444569750 ) ) ;
#1469 = EDGE_LOOP ( 'NONE', ( #23951, #8778, #23474, #3762 ) ) ;
#1470 = ORIENTED_EDGE ( 'NONE', *, *, #18257, .F. ) ;
#1471 = CARTESIAN_POINT ( 'NONE',  ( 1.573500000000000343, -3.414809992080329023E-17, -0.3524999999999999800 ) ) ;
#1472 = CARTESIAN_POINT ( 'NONE',  ( -0.1167790944451424368, 0.5736111110352444253, 0.2819296736111110424 ) ) ;
#1473 = CARTESIAN_POINT ( 'NONE',  ( -1.726321361862525858E-17, 3.852861111186976828, -0.2819296736111110979 ) ) ;
#1474 = CARTESIAN_POINT ( 'NONE',  ( -0.2233192592356399442, 0.1080357141881718996, -0.3073725909049500049 ) ) ;
#1475 = LINE ( 'NONE', #24024, #19713 ) ;
#1476 = CARTESIAN_POINT ( 'NONE',  ( 0.1167790944451424368, 4.495222222298088433, 0.2819296736111110424 ) ) ;
#1477 = DIRECTION ( 'NONE',  ( 0.6123724356957941373, -0.7071067811865463515, -0.3535533905932771725 ) ) ;
#1478 = CARTESIAN_POINT ( 'NONE',  ( -0.1292346314604105872, 4.373694444444443441, -0.3119999999999950591 ) ) ;
#1479 = ORIENTED_EDGE ( 'NONE', *, *, #20943, .T. ) ;
#1480 = VECTOR ( 'NONE', #4022, 39.37007874015748143 ) ;
#1481 = CARTESIAN_POINT ( 'NONE',  ( 0.000000000000000000, 5.072999999999999510, 0.000000000000000000 ) ) ;
#1482 = EDGE_CURVE ( 'NONE', #18107, #16753, #18437, .T. ) ;
#1483 = CARTESIAN_POINT ( 'NONE',  ( -0.2206173157302028232, 3.717444444596176734, -0.2206173157302028232 ) ) ;
#1484 = LINE ( 'NONE', #8793, #21573 ) ;
#1485 = CARTESIAN_POINT ( 'NONE',  ( 2.936000000000001720, 2.740000000000000213, 0.000000000000000000 ) ) ;
#1486 = CARTESIAN_POINT ( 'NONE',  ( 0.3236067977499789694, 0.1785714285714284921, 0.2351141009169893659 ) ) ;
#1487 = CARTESIAN_POINT ( 'NONE',  ( 0.1993543840281267465, 4.929250000075866112, 0.1993543840281266633 ) ) ;
#1488 = DATE_AND_TIME ( #3308, #1403 ) ;
#1489 = DIRECTION ( 'NONE',  ( 0.2813865959466322897, 0.6785357704725523131, 0.6785357704725568651 ) ) ;
#1490 = PLANE ( 'NONE',  #13978 ) ;
#1491 = EDGE_LOOP ( 'NONE', ( #15068, #11395, #22662, #9331 ) ) ;
#1492 = CARTESIAN_POINT ( 'NONE',  ( 0.2819296736111110979, 0.2159722221463555858, 0.000000000000000000 ) ) ;
#1493 = AXIS2_PLACEMENT_3D ( 'NONE', #19854, #21805, #844 ) ;
#1494 = ORIENTED_EDGE ( 'NONE', *, *, #5186, .T. ) ;
#1495 = DIRECTION ( 'NONE',  ( -0.4999999999999916178, 0.000000000000000000, 0.8660254037844434816 ) ) ;
#1496 = DIRECTION ( 'NONE',  ( 0.000000000000000000, 0.000000000000000000, -1.000000000000000000 ) ) ;
#1497 = CARTESIAN_POINT ( 'NONE',  ( -0.3466234456863465652, 4.027014562472920112, 2.644633003996732512 ) ) ;
#1498 = CARTESIAN_POINT ( 'NONE',  ( 2.575339694675500462E-17, -0.01071428571428573000, -0.4205848896953069405 ) ) ;
#1499 = CARTESIAN_POINT ( 'NONE',  ( -0.3119999999999999996, 4.495222222222221120, 0.000000000000000000 ) ) ;
#1500 = CARTESIAN_POINT ( 'NONE',  ( -0.1292346314604032043, 3.762583333333332281, -0.3120000000000024420 ) ) ;
#1501 = FACE_OUTER_BOUND ( 'NONE', #19616, .T. ) ;
#1502 = DIRECTION ( 'NONE',  ( 0.8154147512597614833, -0.5737842049460694094, -0.07661898969830084616 ) ) ;
#1503 = CARTESIAN_POINT ( 'NONE',  ( 0.1993543840281266633, 4.457027777853643791, -0.1993543840281266910 ) ) ;
#1504 = DIRECTION ( 'NONE',  ( 0.000000000000000000, -1.000000000000000000, 1.493785812010397437E-17 ) ) ;
#1505 = CARTESIAN_POINT ( 'NONE',  ( 0.007400005122092102351, 4.543623246078921873, -0.3119247507460371494 ) ) ;
#1506 = CARTESIAN_POINT ( 'NONE',  ( 0.1167790944451424368, 5.161888888964753619, 0.2819296736111110424 ) ) ;
#1507 = CC_DESIGN_PERSON_AND_ORGANIZATION_ASSIGNMENT ( #11185, #18613, ( #11902 ) ) ;
#1508 = CARTESIAN_POINT ( 'NONE',  ( -0.3015329647789626311, 0.05188409045955083565, -0.002760744269507171226 ) ) ;
#1509 = CARTESIAN_POINT ( 'NONE',  ( 0.1920553804271201426, 4.926912892342040884, -0.2492488320715855465 ) ) ;
#1510 = CARTESIAN_POINT ( 'NONE',  ( 0.05498706736770282016, 0.04336109282094929851, 0.2879801573640842216 ) ) ;
#1511 = CARTESIAN_POINT ( 'NONE',  ( -0.4254231800974379030, 0.3089306822179725964, 0.05347271648849764164 ) ) ;
#1512 = CARTESIAN_POINT ( 'NONE',  ( -0.3119999999999999996, 4.279944444596176290, 0.000000000000000000 ) ) ;
#1513 = CARTESIAN_POINT ( 'NONE',  ( 0.1993543840281267465, 4.443138888964754507, 0.1993543840281266633 ) ) ;
#1514 =( BOUNDED_CURVE ( )  B_SPLINE_CURVE ( 2, ( #24064, #7492, #20301, #14938, #20542, #23943, #12887, #9204, #3837 ),
 .UNSPECIFIED., .F., .F. ) 
 B_SPLINE_CURVE_WITH_KNOTS ( ( 3, 2, 2, 2, 3 ),
 ( 0.3645833333333334259, 0.3750000000000000000, 0.3854166666666667407, 0.3958333333333333703, 0.4062499999999999445 ),
 .UNSPECIFIED. ) 
 CURVE ( )  GEOMETRIC_REPRESENTATION_ITEM ( )  RATIONAL_B_SPLINE_CURVE ( ( 0.9999999999999995559, 0.9238795325112871826, 1.000000000000000000, 0.9238795325112867385, 1.000000000000000000, 0.9238795325112867385, 1.000000000000000000, 0.9238795325112871826, 0.9999999999999995559 ) ) 
 REPRESENTATION_ITEM ( '' )  );
#1515 =( BOUNDED_SURFACE ( )  B_SPLINE_SURFACE ( 2, 3, ( 
 ( #22481, #5776, #8957, #5297, #20178, #3465, #10916, #1639, #9074, #23940 ),
 ( #22949, #22839, #17474, #9807, #408, #20891, #17120, #13350, #13712, #9925 ),
 ( #2606, #9558, #8198, #8075, #15411, #5890, #16992, #11758, #21132, #13476 ) ),
 .UNSPECIFIED., .F., .F., .T. ) 
 B_SPLINE_SURFACE_WITH_KNOTS ( ( 3, 3 ),
 ( 4, 3, 3, 4 ),
 ( 0.000000000000000000, 1.000000000000000000 ),
 ( 0.01132290749860156119, 0.02432858112762277536, 0.08935694927272853916, 0.1023626229017496753 ),
 .UNSPECIFIED. ) 
 GEOMETRIC_REPRESENTATION_ITEM ( )  RATIONAL_B_SPLINE_SURFACE ( (
 ( 1.000000000000000000, 1.000000000000000000, 1.000000000000000000, 1.000000000000000000, 1.000000000000000000, 1.000000000000000000, 1.000000000000000000, 1.000000000000000000, 1.000000000000000000, 1.000000000000000000),
 ( 0.4999999999999997780, 0.4999999999999997780, 0.4999999999999997780, 0.4999999999999997780, 0.4999999999999997780, 0.4999999999999997780, 0.4999999999999997780, 0.4999999999999997780, 0.4999999999999997780, 0.4999999999999997780),
 ( 1.000000000000000000, 1.000000000000000000, 1.000000000000000000, 1.000000000000000000, 1.000000000000000000, 1.000000000000000000, 1.000000000000000000, 1.000000000000000000, 1.000000000000000000, 1.000000000000000000) ) ) 
 REPRESENTATION_ITEM ( '' )  SURFACE ( )  );
#1516 = CARTESIAN_POINT ( 'NONE',  ( 0.1167790944451424368, 3.814666666742532630, 0.2819296736111110424 ) ) ;
#1517 = VECTOR ( 'NONE', #7020, 39.37007874015748143 ) ;
#1518 = ORIENTED_EDGE ( 'NONE', *, *, #23286, .T. ) ;
#1519 = VERTEX_POINT ( 'NONE', #20271 ) ;
#1520 = ORIENTED_EDGE ( 'NONE', *, *, #14315, .F. ) ;
#1521 = APPROVAL_STATUS ( 'not_yet_approved' ) ;
#1522 = CARTESIAN_POINT ( 'NONE',  ( -0.3119999999999999996, 4.272999999999998799, 0.000000000000000000 ) ) ;
#1523 = DIRECTION ( 'NONE',  ( -0.7071067811865435759, -0.7071067811865514585, -9.185433182841584085E-17 ) ) ;
#1524 = CARTESIAN_POINT ( 'NONE',  ( -5.731347020009612645E-17, 0.1638888887371559577, 0.3119999999999999996 ) ) ;
#1525 = ADVANCED_FACE ( 'NONE', ( #14674 ), #3439, .T. ) ;
#1526 = VERTEX_POINT ( 'NONE', #9290 ) ;
#1527 = CARTESIAN_POINT ( 'NONE',  ( -0.2206173157302027954, 0.3097222220704892726, -0.2206173157302028232 ) ) ;
#1528 = DIRECTION ( 'NONE',  ( -0.8660254037844377084, 0.000000000000000000, -0.5000000000000015543 ) ) ;
#1529 = CARTESIAN_POINT ( 'NONE',  ( -0.2454434631267384259, 5.121228990971889772, 0.1867560419929801541 ) ) ;
#1530 = DIRECTION ( 'NONE',  ( 0.000000000000000000, 0.000000000000000000, -1.000000000000000000 ) ) ;
#1531 = CARTESIAN_POINT ( 'NONE',  ( 0.1672123529697439048, 0.5028202685342909595, -0.7311626644493618432 ) ) ;
#1532 = ORIENTED_EDGE ( 'NONE', *, *, #12511, .F. ) ;
#1533 = AXIS2_PLACEMENT_3D ( 'NONE', #5580, #13046, #20462 ) ;
#1534 = DIRECTION ( 'NONE',  ( 0.000000000000000000, 1.000000000000000000, 0.000000000000000000 ) ) ;
#1535 = CARTESIAN_POINT ( 'NONE',  ( 0.2764156081756483641, -0.1144950937579611167, 0.2237500000000029743 ) ) ;
#1536 = EDGE_CURVE ( 'NONE', #4238, #3680, #5511, .T. ) ;
#1537 = CARTESIAN_POINT ( 'NONE',  ( -0.2819296736111110979, 4.130638888964754507, 0.000000000000000000 ) ) ;
#1538 = CARTESIAN_POINT ( 'NONE',  ( -0.2819296736111110424, 5.078555555631420582, 0.1167790944451424923 ) ) ;
#1539 = CARTESIAN_POINT ( 'NONE',  ( -0.07411063262681885644, -0.4869405031891911872, 0.4162703459413940599 ) ) ;
#1540 = DIRECTION ( 'NONE',  ( 0.000000000000000000, 0.000000000000000000, 1.000000000000000000 ) ) ;
#1541 = CARTESIAN_POINT ( 'NONE',  ( 0.2206173157302027954, 4.085499999999999687, -0.2206173157302028232 ) ) ;
#1542 = CARTESIAN_POINT ( 'NONE',  ( -0.3119999999999999996, 4.943138889040621820, -0.1292346314604056468 ) ) ;
#1543 = CARTESIAN_POINT ( 'NONE',  ( -0.2819296736111110424, 5.092444444520309865, 0.1167790944451424923 ) ) ;
#1544 = DIRECTION ( 'NONE',  ( 0.000000000000000000, -0.000000000000000000, 1.000000000000000000 ) ) ;
#1545 = CARTESIAN_POINT ( 'NONE',  ( 0.03417713022414695795, 4.683645677618572201, 0.3101606497207352042 ) ) ;
#1546 = VECTOR ( 'NONE', #639, 39.37007874015748854 ) ;
#1547 = CARTESIAN_POINT ( 'NONE',  ( 0.3155070326520292845, -5.795770164686806123E-17, 0.2602083333333368165 ) ) ;
#1548 = CARTESIAN_POINT ( 'NONE',  ( -1.803446527067423865E-16, 0.5196152422706634688, 0.3779506566538943790 ) ) ;
#1549 = ORIENTED_EDGE ( 'NONE', *, *, #9432, .T. ) ;
#1550 = EDGE_CURVE ( 'NONE', #544, #14874, #20510, .T. ) ;
#1551 = CARTESIAN_POINT ( 'NONE',  ( 0.2472135954999579166, 0.03214285714285712581, 0.3402603233408160732 ) ) ;
#1552 = LINE ( 'NONE', #76, #8296 ) ;
#1553 = CARTESIAN_POINT ( 'NONE',  ( 0.2819296736111110424, 0.2124999999241334037, 0.1167790944451424923 ) ) ;
#1554 = CARTESIAN_POINT ( 'NONE',  ( 0.1954553509668047195, 0.1954553509668046085, 0.3522222222222262111 ) ) ;
#1555 = CARTESIAN_POINT ( 'NONE',  ( -0.2819296736111110424, 5.148000000075865223, 0.1167790944451424923 ) ) ;
#1556 = LINE ( 'NONE', #1439, #18274 ) ;
#1557 = EDGE_CURVE ( 'NONE', #3473, #21943, #10774, .T. ) ;
#1558 = ORIENTED_EDGE ( 'NONE', *, *, #22382, .T. ) ;
#1559 = CARTESIAN_POINT ( 'NONE',  ( -0.04084116025059186111, 3.792736021511474487, 0.3120000000000012208 ) ) ;
#1560 = CARTESIAN_POINT ( 'NONE',  ( 2.350334729443114501, -0.003191536374479159947, -2.986000000000000210 ) ) ;
#1561 = CARTESIAN_POINT ( 'NONE',  ( 0.1311510126959312961, 4.873430014960409729, -0.2838723230971368916 ) ) ;
#1562 = CARTESIAN_POINT ( 'NONE',  ( 3.820898013339742174E-17, 5.384999999999999787, 0.3119999999999999996 ) ) ;
#1563 = CARTESIAN_POINT ( 'NONE',  ( -0.2209708691207961095, 0.2209708691207961373, 0.3313888888888925632 ) ) ;
#1564 = CARTESIAN_POINT ( 'NONE',  ( 5.731347020009612645E-17, 4.731333333333332725, 0.3119999999999999996 ) ) ;
#1565 = AXIS2_PLACEMENT_3D ( 'NONE', #1660, #16543, #23964 ) ;
#1566 = CARTESIAN_POINT ( 'NONE',  ( -0.2819296736111110979, 4.016055555631421470, -0.1167790944451422980 ) ) ;
#1567 = CARTESIAN_POINT ( 'NONE',  ( 0.1167790944451424368, 3.773000000075866112, 0.2819296736111110424 ) ) ;
#1568 = CARTESIAN_POINT ( 'NONE',  ( 0.2008485455641423334, 4.022270167221941861, 0.2388045284289016523 ) ) ;
#1569 = CARTESIAN_POINT ( 'NONE',  ( -0.006542161132013071811, 0.5374887588746248834, 0.3892820121258429578 ) ) ;
#1570 = ORIENTED_EDGE ( 'NONE', *, *, #23902, .T. ) ;
#1571 = DIRECTION ( 'NONE',  ( 0.4999999999999942268, 0.000000000000000000, 0.8660254037844420383 ) ) ;
#1572 = CARTESIAN_POINT ( 'NONE',  ( -0.1167790944451423257, 4.453555555631420582, -0.2819296736111110424 ) ) ;
#1573 = CARTESIAN_POINT ( 'NONE',  ( -0.1494206241407597668, 4.511765937384295100, 0.2773182096705338884 ) ) ;
#1574 = CARTESIAN_POINT ( 'NONE',  ( 0.3119999999999998885, 0.07013888888888854256, 0.1292346314604058410 ) ) ;
#1575 = AXIS2_PLACEMENT_3D ( 'NONE', #7907, #4256, #23613 ) ;
#1576 = CARTESIAN_POINT ( 'NONE',  ( 0.2764156081756483641, 0.1144950937579610056, 0.3418055555555594704 ) ) ;
#1577 = AXIS2_PLACEMENT_3D ( 'NONE', #19875, #22301, #2196 ) ;
#1578 = EDGE_CURVE ( 'NONE', #19113, #5067, #18574, .T. ) ;
#1579 = CARTESIAN_POINT ( 'NONE',  ( 0.2819296736111110979, 3.842444444520310309, -0.1167790944451423396 ) ) ;
#1580 = LINE ( 'NONE', #14996, #9950 ) ;
#1581 = CARTESIAN_POINT ( 'NONE',  ( -6.528214817076446933E-07, 5.071585437816050757, 0.3119999999985565986 ) ) ;
#1582 = LINE ( 'NONE', #14762, #16305 ) ;
#1583 = CARTESIAN_POINT ( 'NONE',  ( 0.2923287055106771337, 0.3044642856167432687, -0.2123892367102620249 ) ) ;
#1584 = CARTESIAN_POINT ( 'NONE',  ( 0.1167790944451423535, 0.2472222221463555303, 0.2819296736111110424 ) ) ;
#1585 = CARTESIAN_POINT ( 'NONE',  ( 0.1294417382415924134, 0.3124999999999999445, 0.1612500000000026412 ) ) ;
#1586 = CARTESIAN_POINT ( 'NONE',  ( 0.000000000000000000, 5.384999999999999787, 0.000000000000000000 ) ) ;
#1587 = CARTESIAN_POINT ( 'NONE',  ( -0.01427084424854434090, 0.5924045552181391727, -0.7500000000000002220 ) ) ;
#1588 = CARTESIAN_POINT ( 'NONE',  ( -0.1144950937579609779, 0.2764156081756484196, 0.02236111111111246594 ) ) ;
#1589 = CARTESIAN_POINT ( 'NONE',  ( -0.2764156081756484196, 1.692557448933383907E-17, 0.03972222222222369925 ) ) ;
#1590 = EDGE_CURVE ( 'NONE', #8012, #7081, #24034, .T. ) ;
#1591 = ORIENTED_EDGE ( 'NONE', *, *, #8432, .T. ) ;
#1592 = ORIENTED_EDGE ( 'NONE', *, *, #14489, .T. ) ;
#1593 = DIRECTION ( 'NONE',  ( 0.000000000000000000, 1.000000000000000000, 0.000000000000000000 ) ) ;
#1594 = CARTESIAN_POINT ( 'NONE',  ( 0.000000000000000000, 0.4997679491924311157, 0.2510000000000000009 ) ) ;
#1595 = CARTESIAN_POINT ( 'NONE',  ( 0.3119999999999999996, 0.01805555555555522079, 0.000000000000000000 ) ) ;
#1596 = CARTESIAN_POINT ( 'NONE',  ( -0.1167790944451423535, 3.877166666742531742, 0.2819296736111110424 ) ) ;
#1597 = CARTESIAN_POINT ( 'NONE',  ( -0.1116596296178199582, 0.2473214284738861346, -0.3436530038418508792 ) ) ;
#1598 = ORIENTED_EDGE ( 'NONE', *, *, #18132, .F. ) ;
#1599 = CARTESIAN_POINT ( 'NONE',  ( -0.2819296736111110979, 4.366750000075866112, 0.000000000000000000 ) ) ;
#1600 = CARTESIAN_POINT ( 'NONE',  ( 0.3120000000000000551, 4.963972222222222008, 0.1292346314604056190 ) ) ;
#1601 = CARTESIAN_POINT ( 'NONE',  ( 3.820898013339742174E-17, 5.384999999999999787, 0.3119999999999999996 ) ) ;
#1602 = AXIS2_PLACEMENT_3D ( 'NONE', #22121, #10804, #16647 ) ;
#1603 = ORIENTED_EDGE ( 'NONE', *, *, #21096, .T. ) ;
#1604 = CARTESIAN_POINT ( 'NONE',  ( 0.3119999999999999996, 4.693138888888888971, -0.1292346314604056745 ) ) ;
#1605 = CARTESIAN_POINT ( 'NONE',  ( -0.1292346314604056745, 3.713972222373953525, -0.3119999999999999996 ) ) ;
#1606 = CARTESIAN_POINT ( 'NONE',  ( 0.2581855260733656454, 4.201935345941767430, -0.1757379818918752279 ) ) ;
#1607 = DIRECTION ( 'NONE',  ( 0.000000000000000000, 0.000000000000000000, -1.000000000000000000 ) ) ;
#1608 = CARTESIAN_POINT ( 'NONE',  ( -7.000945310522701902E-17, 0.1678571428571427882, 0.3999999999999999667 ) ) ;
#1609 = CARTESIAN_POINT ( 'NONE',  ( 0.1993543840281267465, 4.707027777853643791, 0.1993543840281266633 ) ) ;
#1610 = ITEM_DEFINED_TRANSFORMATION ( 'NONE', 'NONE', #958,  #9127 ) ;
#1611 = CARTESIAN_POINT ( 'NONE',  ( -0.1543006097263451837, 4.067011077438127842, 0.2711740475169042153 ) ) ;
#1612 = DIRECTION ( 'NONE',  ( 0.000000000000000000, 1.000000000000000000, 0.000000000000000000 ) ) ;
#1613 = CARTESIAN_POINT ( 'NONE',  ( 0.1167790944451423257, 0.3374999999241334314, -0.2819296736111110424 ) ) ;
#1614 = CARTESIAN_POINT ( 'NONE',  ( -5.178964085587577574E-17, 0.2020833332574667185, 0.2819296736111110979 ) ) ;
#1615 = EDGE_CURVE ( 'NONE', #16849, #21333, #8833, .T. ) ;
#1616 = CARTESIAN_POINT ( 'NONE',  ( -0.1292346314604057300, 4.338972222222222008, 0.3119999999999998885 ) ) ;
#1617 = CARTESIAN_POINT ( 'NONE',  ( -0.2340349472341747006, 5.197103598887514941, -0.1654092351966998387 ) ) ;
#1618 = CARTESIAN_POINT ( 'NONE',  ( 0.1236067977499789861, -0.08571428571428572896, -0.3804226065180614236 ) ) ;
#1619 = CARTESIAN_POINT ( 'NONE',  ( 5.731347020009612645E-17, 4.675777777777777366, 0.3119999999999999996 ) ) ;
#1620 = CARTESIAN_POINT ( 'NONE',  ( -1.910449006669871087E-17, 3.759111111111109960, -0.3119999999999999996 ) ) ;
#1621 = CARTESIAN_POINT ( 'NONE',  ( -0.2561990078798795922, 3.885650447666386675, -0.1780621544523601218 ) ) ;
#1622 = FACE_OUTER_BOUND ( 'NONE', #20306, .T. ) ;
#1623 = CARTESIAN_POINT ( 'NONE',  ( -0.1167790944451423257, 4.467444444520309865, -0.2819296736111110424 ) ) ;
#1624 = CARTESIAN_POINT ( 'NONE',  ( -0.3236067977499790249, 0.07678571409062949493, 0.2351141009169892271 ) ) ;
#1625 = CARTESIAN_POINT ( 'NONE',  ( 0.3035782676821786041, 4.527778441137987109, 0.07531847786364795350 ) ) ;
#1626 = CARTESIAN_POINT ( 'NONE',  ( 0.2819296736111110424, 5.175777777853644679, -0.1167790944451423396 ) ) ;
#1627 = DIRECTION ( 'NONE',  ( -0.000000000000000000, -0.000000000000000000, -1.000000000000000000 ) ) ;
#1628 = CARTESIAN_POINT ( 'NONE',  ( 0.3047183941458634915, 3.750271769757703932, 0.06756532177053888033 ) ) ;
#1629 = DIRECTION ( 'NONE',  ( -0.000000000000000000, -1.000000000000000000, -0.000000000000000000 ) ) ;
#1630 = CARTESIAN_POINT ( 'NONE',  ( -0.3255746755405797832, 3.686631053106446565, -0.09499999999999995948 ) ) ;
#1631 = CARTESIAN_POINT ( 'NONE',  ( 0.1292346314604058410, 4.241750000151731648, 0.3119999999999998885 ) ) ;
#1632 = CARTESIAN_POINT ( 'NONE',  ( 5.178964085587577574E-17, 4.547305555631421470, 0.2819296736111110979 ) ) ;
#1633 = CARTESIAN_POINT ( 'NONE',  ( -0.1167790944451423535, 3.752166666742532630, 0.2819296736111110424 ) ) ;
#1634 = EDGE_LOOP ( 'NONE', ( #14741, #21650, #3722 ) ) ;
#1635 = VERTEX_POINT ( 'NONE', #3805 ) ;
#1636 = PERSON_AND_ORGANIZATION_ROLE ( 'design_supplier' ) ;
#1637 = CARTESIAN_POINT ( 'NONE',  ( -0.2206173157302028232, 4.266055555555555046, -0.2206173157302028232 ) ) ;
#1638 = CARTESIAN_POINT ( 'NONE',  ( -0.1568435058878248078, 4.955841575901558826, 0.2727737269072668114 ) ) ;
#1639 = CARTESIAN_POINT ( 'NONE',  ( -0.5116234456863258950, 4.730490217694244492, -2.819759741183656132 ) ) ;
#1640 = ORIENTED_EDGE ( 'NONE', *, *, #14535, .F. ) ;
#1641 = CARTESIAN_POINT ( 'NONE',  ( 1.910449006669871087E-17, 0.3027777776260448528, -0.3119999999999999996 ) ) ;
#1642 = FACE_OUTER_BOUND ( 'NONE', #4880, .T. ) ;
#1643 = CARTESIAN_POINT ( 'NONE',  ( -0.2325997273933552156, 5.121856475730185210, 0.2023777655239332174 ) ) ;
#1644 = CARTESIAN_POINT ( 'NONE',  ( -0.1294417382415922746, -0.3125000000000000000, -0.09569444444444420717 ) ) ;
#1645 = CARTESIAN_POINT ( 'NONE',  ( 0.000000000000000000, 0.000000000000000000, -0.1019043464467004889 ) ) ;
#1646 = ORIENTED_EDGE ( 'NONE', *, *, #19474, .F. ) ;
#1647 = CARTESIAN_POINT ( 'NONE',  ( 0.1116596296178199860, 0.2401785713310289616, -0.3436530038418508792 ) ) ;
#1648 = ORIENTED_EDGE ( 'NONE', *, *, #10070, .T. ) ;
#1649 = CARTESIAN_POINT ( 'NONE',  ( 0.2931105832524772969, 5.082463614296739429, 0.1082669822925051151 ) ) ;
#1650 = CARTESIAN_POINT ( 'NONE',  ( -0.1954553509668046918, -0.1954553509668046640, 0.2619444444444477549 ) ) ;
#1651 = CARTESIAN_POINT ( 'NONE',  ( -0.1993543840281266910, 4.179250000075865223, -0.1993543840281266910 ) ) ;
#1652 = CARTESIAN_POINT ( 'NONE',  ( 0.1167790944451424506, 5.148000000075865223, 0.2819296736111110424 ) ) ;
#1653 = CARTESIAN_POINT ( 'NONE',  ( -0.4687500000000003886, 0.2170121405309672902, 0.07051002209705402313 ) ) ;
#1654 = CARTESIAN_POINT ( 'NONE',  ( -0.2990811592642881878, 4.226951744488065543, 0.09065860205554784890 ) ) ;
#1655 = CARTESIAN_POINT ( 'NONE',  ( 0.3119999999999999996, 3.963972222222221564, 0.1292346314604056190 ) ) ;
#1656 = CARTESIAN_POINT ( 'NONE',  ( 0.3119999999999999996, 4.915361111262843252, 0.1292346314604056190 ) ) ;
#1657 = VECTOR ( 'NONE', #16201, 39.37007874015748854 ) ;
#1658 = CARTESIAN_POINT ( 'NONE',  ( 0.2819296736111111534, 5.057722222298088433, 0.1167790944451422563 ) ) ;
#1659 = EDGE_CURVE ( 'NONE', #409, #2709, #12359, .T. ) ;
#1660 = CARTESIAN_POINT ( 'NONE',  ( 0.000000000000000000, 0.000000000000000000, 1.326383476483184332 ) ) ;
#1661 = VERTEX_POINT ( 'NONE', #21854 ) ;
#1662 = CARTESIAN_POINT ( 'NONE',  ( 0.2236587330425323095, -0.2167494423012602534, 0.4226684177326948677 ) ) ;
#1663 = CARTESIAN_POINT ( 'NONE',  ( -0.2056020336012781280, 0.05660050360928185753, 0.2269839081635093292 ) ) ;
#1664 = EDGE_LOOP ( 'NONE', ( #16964, #17985, #11126, #20437 ) ) ;
#1665 = ADVANCED_FACE ( 'NONE', ( #1976 ), #5143, .F. ) ;
#1666 = CARTESIAN_POINT ( 'NONE',  ( -0.1306872919485615459, -0.3155070326520293400, 0.3539583333333376491 ) ) ;
#1667 = CARTESIAN_POINT ( 'NONE',  ( 0.1167790944451422702, 5.168833333409199149, -0.2819296736111110424 ) ) ;
#1668 = TOROIDAL_SURFACE ( 'NONE', #18418, 0.6209078282299125284, 0.01874999999999999931 ) ;
#1669 = CARTESIAN_POINT ( 'NONE',  ( 0.2688280863486493533, -0.3751924628947166940, 0.4334272443489663451 ) ) ;
#1670 = CARTESIAN_POINT ( 'NONE',  ( 0.000000000000000000, 5.384999999999999787, -0.3119999999999999996 ) ) ;
#1671 = CARTESIAN_POINT ( 'NONE',  ( 0.1993543840281266355, 0.2645833332574666907, 0.1993543840281267465 ) ) ;
#1672 = CARTESIAN_POINT ( 'NONE',  ( -3.385114897866767815E-17, -0.2764156081756484196, 0.1647222222222247123 ) ) ;
#1673 = CARTESIAN_POINT ( 'NONE',  ( 0.1993543840281267465, 5.165361111186976828, 0.1993543840281266633 ) ) ;
#1674 = LINE ( 'NONE', #20214, #21390 ) ;
#1675 = EDGE_LOOP ( 'NONE', ( #3593, #18958, #2487, #18412, #23544 ) ) ;
#1676 = CARTESIAN_POINT ( 'NONE',  ( -0.1167790944451423535, 4.807722222298087544, 0.2819296736111110424 ) ) ;
#1677 = CARTESIAN_POINT ( 'NONE',  ( -0.2724619974122192700, 4.164101067513843901, -0.1574067719271113330 ) ) ;
#1678 = DIRECTION ( 'NONE',  ( 0.000000000000000000, -0.9961946980917454342, 0.08715574274765833240 ) ) ;
#1679 = CARTESIAN_POINT ( 'NONE',  ( -0.5116234456863466562, 1.808198851485059100, 2.664840263418369659 ) ) ;
#1680 = CARTESIAN_POINT ( 'NONE',  ( -0.4805070082343984583, 0.2560807851245828770, 0.04413116910601658921 ) ) ;
#1681 = CARTESIAN_POINT ( 'NONE',  ( 0.3119999999999999996, 4.634111111111110404, -3.820898013339742174E-17 ) ) ;
#1682 = CARTESIAN_POINT ( 'NONE',  ( -0.2819296736111110979, 3.960500000075865668, -0.1167790944451422980 ) ) ;
#1683 = CARTESIAN_POINT ( 'NONE',  ( -1.726321361862525858E-17, 3.741750000075865668, -0.2819296736111110979 ) ) ;
#1684 = CARTESIAN_POINT ( 'NONE',  ( 0.2591841582727462123, 4.035241130471740156, -0.1755254409656935577 ) ) ;
#1685 = CARTESIAN_POINT ( 'NONE',  ( 0.01298578716746627733, 0.5473886244374734922, 0.04271891838948498055 ) ) ;
#1686 = VERTEX_POINT ( 'NONE', #16377 ) ;
#1687 = DIRECTION ( 'NONE',  ( 0.000000000000000000, 1.000000000000000000, 0.000000000000000000 ) ) ;
#1688 = EDGE_LOOP ( 'NONE', ( #15767, #21825, #18890, #22350 ) ) ;
#1689 = ADVANCED_FACE ( 'NONE', ( #23788 ), #18318, .T. ) ;
#1690 = CARTESIAN_POINT ( 'NONE',  ( 5.178964085587577574E-17, 4.311194444520309865, 0.2819296736111110979 ) ) ;
#1691 = DIRECTION ( 'NONE',  ( 0.000000000000000000, 1.000000000000000000, 0.000000000000000000 ) ) ;
#1692 = EDGE_CURVE ( 'NONE', #6549, #4536, #5723, .T. ) ;
#1693 = DIRECTION ( 'NONE',  ( -1.000000000000000000, 0.000000000000000000, 0.000000000000000000 ) ) ;
#1694 = CARTESIAN_POINT ( 'NONE',  ( -0.2764156081756484196, 0.1144950937579609918, 0.3070833333333369830 ) ) ;
#1695 = CARTESIAN_POINT ( 'NONE',  ( -0.1166234456863465552, 0.9548081934128058723, 2.711183489075826181 ) ) ;
#1696 = DIRECTION ( 'NONE',  ( -0.000000000000000000, 1.000000000000000000, -0.000000000000000000 ) ) ;
#1697 = CARTESIAN_POINT ( 'NONE',  ( 0.3308333333333332571, 3.738758431839877614E-19, 0.4425000000000000044 ) ) ;
#1698 = CARTESIAN_POINT ( 'NONE',  ( -0.1116596296178199582, 0.2473214284738861346, -0.3436530038418508792 ) ) ;
#1699 = CARTESIAN_POINT ( 'NONE',  ( 0.2819296736111110424, 0.2611111110352444808, -0.1167790944451423119 ) ) ;
#1700 = CARTESIAN_POINT ( 'NONE',  ( -3.268767525105149064E-07, 3.877166675600695722, -0.3119999999998287477 ) ) ;
#1701 = CARTESIAN_POINT ( 'NONE',  ( -5.731347020009612645E-17, 0.5597222222222218990, 0.3119999999999999996 ) ) ;
#1702 = FACE_OUTER_BOUND ( 'NONE', #19122, .T. ) ;
#1703 = CARTESIAN_POINT ( 'NONE',  ( -0.1954553509668046640, 0.1954553509668046918, -0.1338888888888887796 ) ) ;
#1704 = VECTOR ( 'NONE', #8060, 39.37007874015748143 ) ;
#1705 = ORIENTED_EDGE ( 'NONE', *, *, #18713, .F. ) ;
#1706 = EDGE_LOOP ( 'NONE', ( #20611, #10289, #4801, #22116 ) ) ;
#1707 = CARTESIAN_POINT ( 'NONE',  ( -0.1888797109280974940, 5.097681916776925171, -0.2473108602307070025 ) ) ;
#1708 = DIRECTION ( 'NONE',  ( 0.000000000000000000, 0.000000000000000000, -1.000000000000000000 ) ) ;
#1709 = CARTESIAN_POINT ( 'NONE',  ( 1.726321361862525858E-17, 0.6048611110352445364, -0.2819296736111110979 ) ) ;
#1710 = CARTESIAN_POINT ( 'NONE',  ( -0.1167790944451423535, 3.932722222298087544, 0.2819296736111110424 ) ) ;
#1711 = CARTESIAN_POINT ( 'NONE',  ( -0.2923287055106771337, 0.1973214284738861179, 0.2123892367102619971 ) ) ;
#1712 = CARTESIAN_POINT ( 'NONE',  ( 0.1993543840281266633, 4.345916666742532186, -0.1993543840281266910 ) ) ;
#1713 = DIRECTION ( 'NONE',  ( -0.8660254037844437036, 0.000000000000000000, -0.4999999999999913403 ) ) ;
#1714 = CARTESIAN_POINT ( 'NONE',  ( 0.000000000000000000, 5.384999999999999787, -0.3119999999999999996 ) ) ;
#1715 = VERTEX_POINT ( 'NONE', #2091 ) ;
#1716 = ADVANCED_FACE ( 'NONE', ( #5984 ), #10027, .T. ) ;
#1717 = DIRECTION ( 'NONE',  ( 0.5000000000000003331, 0.000000000000000000, -0.8660254037844383745 ) ) ;
#1718 = CARTESIAN_POINT ( 'NONE',  ( -0.2819296736111110424, 4.856333333409198261, 0.1167790944451424923 ) ) ;
#1719 = CARTESIAN_POINT ( 'NONE',  ( 0.2730705943700247329, 4.192115419233818585, 0.1511490652758342157 ) ) ;
#1720 = CIRCLE ( 'NONE', #7177, 0.3425000000000000266 ) ;
#1721 = EDGE_CURVE ( 'NONE', #23820, #20507, #6226, .T. ) ;
#1722 = CARTESIAN_POINT ( 'NONE',  ( 0.3149999999999997802, 0.06786299768266475241, -3.857637417314159607E-17 ) ) ;
#1723 = APPLICATION_CONTEXT ( 'configuration controlled 3d designs of mechanical parts and assemblies' ) ;
#1724 = CARTESIAN_POINT ( 'NONE',  ( -0.1993543840281266355, 4.582027777853642903, 0.1993543840281267465 ) ) ;
#1725 = VERTEX_POINT ( 'NONE', #4038 ) ;
#1726 = CARTESIAN_POINT ( 'NONE',  ( -0.4570242136016682832, 0.2774028246161723832, 0.04874733047934379920 ) ) ;
#1727 = CARTESIAN_POINT ( 'NONE',  ( -1.889944503261478141E-16, 0.5289902422706634910, 0.3941886329748526263 ) ) ;
#1728 = CARTESIAN_POINT ( 'NONE',  ( -0.1167790944451422702, 0.5111111110352446474, -0.2819296736111110424 ) ) ;
#1729 = ORIENTED_EDGE ( 'NONE', *, *, #1812, .T. ) ;
#1730 = ORIENTED_EDGE ( 'NONE', *, *, #2615, .T. ) ;
#1731 = CARTESIAN_POINT ( 'NONE',  ( 0.2819296736111110424, 0.1638888888130222432, -0.1167790944451423119 ) ) ;
#1732 = CARTESIAN_POINT ( 'NONE',  ( -0.1655462978948334940, 4.715401455808697406, -0.2649287660789821919 ) ) ;
#1733 = CARTESIAN_POINT ( 'NONE',  ( -0.4500000000000003997, -0.2598076211353319009, 0.3779506566538942125 ) ) ;
#1734 = CARTESIAN_POINT ( 'NONE',  ( -0.2472135954999579444, -0.003571428571428599073, -0.3402603233408159622 ) ) ;
#1735 = DIRECTION ( 'NONE',  ( 0.000000000000000000, 0.000000000000000000, 1.000000000000000000 ) ) ;
#1736 = EDGE_CURVE ( 'NONE', #1821, #24062, #11611, .T. ) ;
#1737 = CARTESIAN_POINT ( 'NONE',  ( -0.2620303320828955007, 3.885945015255288126, -0.1694884108109906695 ) ) ;
#1738 = CARTESIAN_POINT ( 'NONE',  ( 1.069687032369026403, 2.453197021783230625, -1.096034709530573359 ) ) ;
#1739 = CARTESIAN_POINT ( 'NONE',  ( 0.2819296736111110979, 4.450083333409199149, -3.452642723725051716E-17 ) ) ;
#1740 = CARTESIAN_POINT ( 'NONE',  ( 0.3236067977499790249, -0.03035714305222763157, -0.2351141009169892826 ) ) ;
#1741 = CARTESIAN_POINT ( 'NONE',  ( -0.1292346314604056190, 0.2506944442927114824, -0.3119999999999999996 ) ) ;
#1742 = AXIS2_PLACEMENT_3D ( 'NONE', #5975, #23036, #13317 ) ;
#1743 = CARTESIAN_POINT ( 'NONE',  ( 0.2819296736111110424, 5.064666666742533074, -0.1167790944451423396 ) ) ;
#1744 = CARTESIAN_POINT ( 'NONE',  ( 0.1167790944451422702, 4.391055555631420582, -0.2819296736111110979 ) ) ;
#1745 = CARTESIAN_POINT ( 'NONE',  ( 0.1573838318022541261, 3.761421851761045154, -0.2699628318548333850 ) ) ;
#1746 = CARTESIAN_POINT ( 'NONE',  ( -5.731347020009612645E-17, 0.4972222220704892726, 0.3119999999999999996 ) ) ;
#1747 = CARTESIAN_POINT ( 'NONE',  ( -0.3394572874457115752, 3.700000000000000622, -0.09499999999999993172 ) ) ;
#1748 = CARTESIAN_POINT ( 'NONE',  ( -0.1292346314604056745, 4.102861111262843252, -0.3119999999999999996 ) ) ;
#1749 = CARTESIAN_POINT ( 'NONE',  ( 0.1167790944451424506, 4.495222222298088433, 0.2819296736111110424 ) ) ;
#1750 = LOCAL_TIME ( 21, 9, 13.00000000000000000, #1455 ) ;
#1751 = CARTESIAN_POINT ( 'NONE',  ( 0.2819296736111110979, 3.932722222298087544, 0.1167790944451422425 ) ) ;
#1752 = VERTEX_POINT ( 'NONE', #2579 ) ;
#1753 = ORIENTED_EDGE ( 'NONE', *, *, #10794, .F. ) ;
#1754 = PERSON_AND_ORGANIZATION ( #15518, #2538 ) ;
#1755 = CARTESIAN_POINT ( 'NONE',  ( -0.1484667313405303724, -0.2653928060427109825, 0.4153036484830501807 ) ) ;
#1756 = AXIS2_PLACEMENT_3D ( 'NONE', #13765, #2772, #12189 ) ;
#1757 = FACE_OUTER_BOUND ( 'NONE', #2089, .T. ) ;
#1758 = EDGE_LOOP ( 'NONE', ( #14412, #12025, #21999, #8230 ) ) ;
#1759 = CARTESIAN_POINT ( 'NONE',  ( 0.1292346314604057023, 0.3895833331816003775, 0.3119999999999998885 ) ) ;
#1760 = CARTESIAN_POINT ( 'NONE',  ( 0.2730879860166530726, 0.9548081934128058723, 2.751417548891517573 ) ) ;
#1761 = DIRECTION ( 'NONE',  ( 0.000000000000000000, 0.000000000000000000, 1.000000000000000000 ) ) ;
#1762 = FACE_OUTER_BOUND ( 'NONE', #21500, .T. ) ;
#1763 = CARTESIAN_POINT ( 'NONE',  ( 0.1919009159517996166, 3.982454885862982685, -0.2493777159950087974 ) ) ;
#1764 = EDGE_LOOP ( 'NONE', ( #12031, #20826, #727, #18229, #8979, #5602, #22234, #9828, #12167, #16375 ) ) ;
#1765 = LOCAL_TIME ( 21, 9, 13.00000000000000000, #20534 ) ;
#1766 = CARTESIAN_POINT ( 'NONE',  ( -0.2233192592356400275, 0.05803571418817188299, 0.3073725909049499494 ) ) ;
#1767 = ORIENTED_EDGE ( 'NONE', *, *, #23255, .F. ) ;
#1768 = CARTESIAN_POINT ( 'NONE',  ( 0.3114906597041430802, 5.086078164599575402, -0.01551821721983479528 ) ) ;
#1769 = CARTESIAN_POINT ( 'NONE',  ( -0.2764156081756484196, 1.692557448933383907E-17, 0.3105555555555591929 ) ) ;
#1770 = CARTESIAN_POINT ( 'NONE',  ( 0.2819296736111110979, 4.213972222298087544, -3.452642723725051716E-17 ) ) ;
#1771 = CARTESIAN_POINT ( 'NONE',  ( -0.1167790944451423119, 5.120222222298088433, -0.2819296736111110979 ) ) ;
#1772 = CARTESIAN_POINT ( 'NONE',  ( -0.009374999999999756792, -0.5358532185916218271, 0.3779506566538943235 ) ) ;
#1773 = CARTESIAN_POINT ( 'NONE',  ( 1.910449006669871087E-17, 0.3583333331816003775, -0.3119999999999999996 ) ) ;
#1774 = CARTESIAN_POINT ( 'NONE',  ( 0.3806690758928571450, 0.4111607142369430590, 0.000000000000000000 ) ) ;
#1775 = CARTESIAN_POINT ( 'NONE',  ( 5.731347020009612645E-17, 4.904944444596176290, 0.3119999999999999996 ) ) ;
#1776 = VECTOR ( 'NONE', #21022, 39.37007874015748854 ) ;
#1777 = CARTESIAN_POINT ( 'NONE',  ( 0.3039826620300027926, 4.805727411070424893, 0.07105243237910956189 ) ) ;
#1778 = DIRECTION ( 'NONE',  ( 0.000000000000000000, 0.000000000000000000, -1.000000000000000000 ) ) ;
#1779 = DIRECTION ( 'NONE',  ( 0.8651979924482661177, -0.04370253788966847047, -0.4995222938423191650 ) ) ;
#1780 = EDGE_CURVE ( 'NONE', #23361, #1879, #11797, .T. ) ;
#1781 = CC_DESIGN_SECURITY_CLASSIFICATION ( #7632, ( #24129 ) ) ;
#1782 = CARTESIAN_POINT ( 'NONE',  ( 0.000000000000000000, 3.738758431839877614E-19, 0.4425000000000000044 ) ) ;
#1783 = ORIENTED_EDGE ( 'NONE', *, *, #12175, .T. ) ;
#1784 = CARTESIAN_POINT ( 'NONE',  ( -0.1306872919485615459, -0.3155070326520293400, 0.2984027777777815138 ) ) ;
#1785 = CARTESIAN_POINT ( 'NONE',  ( 0.1993543840281267465, 5.151472222298087544, 0.1993543840281266633 ) ) ;
#1786 = VECTOR ( 'NONE', #10880, 39.37007874015747433 ) ;
#1787 = AXIS2_PLACEMENT_3D ( 'NONE', #13488, #19074, #18716 ) ;
#1788 = CARTESIAN_POINT ( 'NONE',  ( 0.3999999999999999667, 0.03928571428571425023, 0.1299678784931626307 ) ) ;
#1789 = DIRECTION ( 'NONE',  ( -0.000000000000000000, -1.000000000000000000, -0.000000000000000000 ) ) ;
#1790 = CARTESIAN_POINT ( 'NONE',  ( 0.1167790944451423535, 0.2611111110352444808, 0.2819296736111110979 ) ) ;
#1791 = CARTESIAN_POINT ( 'NONE',  ( -0.2764156081756484196, -0.1144950937579609362, 0.2098611111111139405 ) ) ;
#1792 = CARTESIAN_POINT ( 'NONE',  ( 0.2819296736111110979, 5.002166666742532186, 0.1167790944451422425 ) ) ;
#1793 = ORIENTED_EDGE ( 'NONE', *, *, #14324, .F. ) ;
#1794 = CARTESIAN_POINT ( 'NONE',  ( 0.1993543840281267465, 4.984805555631420582, 0.1993543840281266633 ) ) ;
#1795 = DIRECTION ( 'NONE',  ( -0.000000000000000000, -1.000000000000000000, -0.000000000000000000 ) ) ;
#1796 = DIRECTION ( 'NONE',  ( 0.000000000000000000, 0.000000000000000000, 1.000000000000000000 ) ) ;
#1797 = DIRECTION ( 'NONE',  ( -0.4999999999999877320, 0.000000000000000000, 0.8660254037844458130 ) ) ;
#1798 = LINE ( 'NONE', #12801, #287 ) ;
#1799 = CARTESIAN_POINT ( 'NONE',  ( 0.1292346314604058410, 4.401472222222221120, 0.3119999999999998885 ) ) ;
#1800 = CARTESIAN_POINT ( 'NONE',  ( 0.1993543840281266633, 4.054250000075865223, -0.1993543840281266910 ) ) ;
#1801 = CARTESIAN_POINT ( 'NONE',  ( 4.898587196589413075E-17, 3.700000000000000622, 0.4000000000000000222 ) ) ;
#1802 = CARTESIAN_POINT ( 'NONE',  ( 0.05402694832707571893, 4.042351412354395990, -0.3076319426930580470 ) ) ;
#1803 = CARTESIAN_POINT ( 'NONE',  ( -0.01172578639831981309, 0.5344959914317445326, 0.04874733047933996199 ) ) ;
#1804 = VECTOR ( 'NONE', #6422, 39.37007874015748854 ) ;
#1805 = LINE ( 'NONE', #18392, #19451 ) ;
#1806 = LINE ( 'NONE', #13175, #1362 ) ;
#1807 = CARTESIAN_POINT ( 'NONE',  ( 0.3114133620982494355, 4.640484927562076756, 0.02096553565331283828 ) ) ;
#1808 = CARTESIAN_POINT ( 'NONE',  ( -0.2764156081756484196, -0.1144950937579609362, 0.2029166666666694652 ) ) ;
#1809 = DIRECTION ( 'NONE',  ( -1.000000000000000000, 0.000000000000000000, 0.000000000000000000 ) ) ;
#1810 = CARTESIAN_POINT ( 'NONE',  ( -0.08089845032000375635, 4.435061056889780140, -0.3020206211261280971 ) ) ;
#1811 = CARTESIAN_POINT ( 'NONE',  ( 0.01571427698143865528, -0.5457913482617615664, 0.04342012612512788361 ) ) ;
#1812 = EDGE_CURVE ( 'NONE', #16762, #4265, #19042, .T. ) ;
#1813 = CARTESIAN_POINT ( 'NONE',  ( 0.3613381517857143232, 0.2223214284738861402, 0.1174058825155742114 ) ) ;
#1814 = AXIS2_PLACEMENT_3D ( 'NONE', #4160, #18796, #5754 ) ;
#1815 = CARTESIAN_POINT ( 'NONE',  ( 0.1167790944451423257, 0.1569444443685778234, -0.2819296736111110424 ) ) ;
#1816 = CARTESIAN_POINT ( 'NONE',  ( -0.1294417382415922191, 0.3125000000000000000, 0.1681944444444471720 ) ) ;
#1817 = DIRECTION ( 'NONE',  ( 0.000000000000000000, -0.5150380749100549327, -0.8571673007021117785 ) ) ;
#1818 = CARTESIAN_POINT ( 'NONE',  ( 0.1964672255785170629, 0.4278354717905788474, 0.4172182224143142215 ) ) ;
#1819 = CARTESIAN_POINT ( 'NONE',  ( -0.1954553509668046640, 0.1954553509668046918, -0.07833333333333279691 ) ) ;
#1820 = ORIENTED_EDGE ( 'NONE', *, *, #21215, .F. ) ;
#1821 = VERTEX_POINT ( 'NONE', #9533 ) ;
#1822 = CARTESIAN_POINT ( 'NONE',  ( -0.2689956684658347807, 5.109708706941876066, 0.1540837381399228490 ) ) ;
#1823 = DIRECTION ( 'NONE',  ( -0.000000000000000000, -1.000000000000000000, -0.000000000000000000 ) ) ;
#1824 = CARTESIAN_POINT ( 'NONE',  ( 0.2206173157302028232, 0.02499999999999966485, -0.2206173157302028232 ) ) ;
#1825 = CARTESIAN_POINT ( 'NONE',  ( -0.2819296736111110979, 3.866750000075866112, 0.000000000000000000 ) ) ;
#1826 = CARTESIAN_POINT ( 'NONE',  ( 0.1116596296178199027, 0.2116071427596004639, 0.3436530038418508792 ) ) ;
#1827 = ADVANCED_FACE ( 'NONE', ( #9900 ), #22693, .T. ) ;
#1828 = CARTESIAN_POINT ( 'NONE',  ( 0.1993543840281266633, 4.512583333409199149, -0.1993543840281266910 ) ) ;
#1829 = CYLINDRICAL_SURFACE ( 'NONE', #13178, 0.3119999999999999996 ) ;
#1830 = PLANE ( 'NONE',  #2830 ) ;
#1831 = ORIENTED_EDGE ( 'NONE', *, *, #16016, .T. ) ;
#1832 = CARTESIAN_POINT ( 'NONE',  ( 1.131433074307491404, 3.066692553488282957, 0.8537320438460626049 ) ) ;
#1833 = CARTESIAN_POINT ( 'NONE',  ( -1.726321361862525858E-17, 5.061194444520309865, -0.2819296736111110979 ) ) ;
#1834 = CARTESIAN_POINT ( 'NONE',  ( -0.01961490578657244105, 5.143841740609819801, -0.3033781769544516838 ) ) ;
#1835 = AXIS2_PLACEMENT_3D ( 'NONE', #20819, #4347, #2046 ) ;
#1836 = CARTESIAN_POINT ( 'NONE',  ( 5.096684635251240714, -0.7749801676295677844, -2.474376554313653109 ) ) ;
#1837 = CARTESIAN_POINT ( 'NONE',  ( 0.4000000000000000222, 0.2482142855192008835, 0.000000000000000000 ) ) ;
#1838 = CARTESIAN_POINT ( 'NONE',  ( 0.2472135954999579166, 0.1749999999999999889, 0.3402603233408160732 ) ) ;
#1839 = CARTESIAN_POINT ( 'NONE',  ( 0.1167790944451422702, 4.724388888964754507, -0.2819296736111110979 ) ) ;
#1840 = CARTESIAN_POINT ( 'NONE',  ( -0.3119999999999998885, 4.776472222222222008, 0.1292346314604058410 ) ) ;
#1841 = CARTESIAN_POINT ( 'NONE',  ( 1.910449006669871087E-17, 0.4138888887371559577, -0.3119999999999999996 ) ) ;
#1842 = CARTESIAN_POINT ( 'NONE',  ( -0.2819296736111110979, 0.5249999999241332649, 0.1167790944451422425 ) ) ;
#1843 = ADVANCED_FACE ( 'NONE', ( #15266 ), #11492, .F. ) ;
#1844 = ORIENTED_EDGE ( 'NONE', *, *, #7479, .F. ) ;
#1845 = ORIENTED_EDGE ( 'NONE', *, *, #3639, .T. ) ;
#1846 = CARTESIAN_POINT ( 'NONE',  ( 0.1993543840281266355, 0.1534722221463556135, 0.1993543840281267465 ) ) ;
#1847 = DIRECTION ( 'NONE',  ( 0.7071067811865474617, -0.000000000000000000, -0.7071067811865474617 ) ) ;
#1848 = CARTESIAN_POINT ( 'NONE',  ( -0.06335377612981410445, 0.3713837754639563449, 0.4000000000000001887 ) ) ;
#1849 = CARTESIAN_POINT ( 'NONE',  ( 0.4000000000000000222, 0.1857142857142856651, 0.000000000000000000 ) ) ;
#1850 = CARTESIAN_POINT ( 'NONE',  ( 0.2230971623002953874, -0.2230971623002954429, -0.02798611111111037192 ) ) ;
#1851 = LINE ( 'NONE', #16735, #1704 ) ;
#1852 = CARTESIAN_POINT ( 'NONE',  ( -0.2912517187485964554, 3.894337629471870788, 0.1144103805008772345 ) ) ;
#1853 = CARTESIAN_POINT ( 'NONE',  ( 0.2819296736111110979, 0.3166666665908000056, -0.1167790944451422980 ) ) ;
#1854 = CARTESIAN_POINT ( 'NONE',  ( -0.2819296736111110424, 0.05972222214635559273, -0.1167790944451423396 ) ) ;
#1855 = CARTESIAN_POINT ( 'NONE',  ( -0.1167790944451423257, 4.578555555631421470, -0.2819296736111110424 ) ) ;
#1856 = AXIS2_PLACEMENT_3D ( 'NONE', #4592, #6657, #12051 ) ;
#1857 = CARTESIAN_POINT ( 'NONE',  ( 0.2472135954999579721, -0.02678571448079906589, -0.3402603233408159622 ) ) ;
#1858 = CARTESIAN_POINT ( 'NONE',  ( 4.113055369932088708E-16, 0.1589285712334866096, 0.4000000000000000222 ) ) ;
#1859 = EDGE_CURVE ( 'NONE', #13713, #9037, #17449, .T. ) ;
#1860 = CARTESIAN_POINT ( 'NONE',  ( 0.1993543840281266633, 5.012583333409199149, -0.1993543840281266910 ) ) ;
#1861 = SHAPE_REPRESENTATION ( 'Aloris-BXA-Top-Bushing', ( #9127 ), #2886 ) ;
#1862 = CARTESIAN_POINT ( 'NONE',  ( 0.2819296736111110979, 4.547305555631421470, -3.452642723725051716E-17 ) ) ;
#1863 = CARTESIAN_POINT ( 'NONE',  ( 0.000000000000000000, 5.384999999999999787, 0.000000000000000000 ) ) ;
#1864 = PERSON ( 'NAUO-PER8', 'UNSPECIFIED', 'UNSPECIFIED', ('UNSPECIFIED'), ('UNSPECIFIED'), ('UNSPECIFIED') ) ;
#1865 = CARTESIAN_POINT ( 'NONE',  ( 0.000000000000000000, 0.9040586665785882436, 0.000000000000000000 ) ) ;
#1866 = CARTESIAN_POINT ( 'NONE',  ( 0.04950202671021954742, 3.931318200535246277, -0.3090077374095805962 ) ) ;
#1867 = CARTESIAN_POINT ( 'NONE',  ( 0.1292346314604056190, 3.984805555707287894, -0.3119999999999999996 ) ) ;
#1868 = CARTESIAN_POINT ( 'NONE',  ( -0.1167790944451423119, 4.578555555631421470, -0.2819296736111110979 ) ) ;
#1869 = CARTESIAN_POINT ( 'NONE',  ( -0.06335377612981410445, 0.2999552040353848925, 0.4000000000000001887 ) ) ;
#1870 = ORIENTED_EDGE ( 'NONE', *, *, #19160, .T. ) ;
#1871 = LINE ( 'NONE', #7600, #3677 ) ;
#1872 = ORIENTED_EDGE ( 'NONE', *, *, #18577, .F. ) ;
#1873 = AXIS2_PLACEMENT_3D ( 'NONE', #18586, #7606, #18345 ) ;
#1874 = ORIENTED_EDGE ( 'NONE', *, *, #12510, .F. ) ;
#1875 = APPROVAL_DATE_TIME ( #16519, #16403 ) ;
#1876 = CARTESIAN_POINT ( 'NONE',  ( 1.658214884748263618, 0.000000000000000000, -2.174029041877829638 ) ) ;
#1877 = CARTESIAN_POINT ( 'NONE',  ( 0.000000000000000000, 3.738758431839877614E-19, 0.4425000000000000044 ) ) ;
#1878 = FACE_OUTER_BOUND ( 'NONE', #4340, .T. ) ;
#1879 = VERTEX_POINT ( 'NONE', #7932 ) ;
#1880 = CARTESIAN_POINT ( 'NONE',  ( 0.1292346314604056745, 0.5770833331816004330, -0.3119999999999999996 ) ) ;
#1881 = ORIENTED_EDGE ( 'NONE', *, *, #22586, .T. ) ;
#1882 = CARTESIAN_POINT ( 'NONE',  ( -4.638126268221291196E-16, 0.1232142855192009251, -0.4000000000000000222 ) ) ;
#1883 = CARTESIAN_POINT ( 'NONE',  ( -0.2034396455339492205, 3.716810070265228028, -0.2365585480272117402 ) ) ;
#1884 = CARTESIAN_POINT ( 'NONE',  ( -0.4687500000000002220, 0.2630787017013380136, 0.3892820121258430133 ) ) ;
#1885 = CARTESIAN_POINT ( 'NONE',  ( 0.04088039599977719152, 3.987110618275341523, -0.3119999999999992779 ) ) ;
#1886 = ORIENTED_EDGE ( 'NONE', *, *, #11812, .T. ) ;
#1887 = CARTESIAN_POINT ( 'NONE',  ( 0.2233192592356399164, 0.1437499999024575703, 0.3073725909049500604 ) ) ;
#1888 = ORIENTED_EDGE ( 'NONE', *, *, #16334, .F. ) ;
#1889 = PLANE ( 'NONE',  #13473 ) ;
#1890 = CARTESIAN_POINT ( 'NONE',  ( -0.2764156081756484196, -0.1144950937579609362, 0.3140277777777815138 ) ) ;
#1891 = EDGE_CURVE ( 'NONE', #6978, #18107, #6506, .T. ) ;
#1892 = CARTESIAN_POINT ( 'NONE',  ( 0.2819296736111110979, 4.269527777853643791, -3.452642723725051716E-17 ) ) ;
#1893 = CARTESIAN_POINT ( 'NONE',  ( 0.1993543840281267465, 5.040361111186975940, 0.1993543840281266633 ) ) ;
#1894 = CARTESIAN_POINT ( 'NONE',  ( -0.04549985820534920705, -0.5149965219823262608, 0.3899922761138021055 ) ) ;
#1895 = DIRECTION ( 'NONE',  ( 0.5000000000000012212, 0.8660254037844380415, -1.821231995776176268E-15 ) ) ;
#1896 = CARTESIAN_POINT ( 'NONE',  ( -0.3119999999999998885, 3.776472222222221564, 0.1292346314604058410 ) ) ;
#1897 = AXIS2_PLACEMENT_3D ( 'NONE', #4811, #12278, #19694 ) ;
#1898 = CARTESIAN_POINT ( 'NONE',  ( -1.910449006669871087E-17, 4.766055555707287894, -0.3119999999999999996 ) ) ;
#1899 = CARTESIAN_POINT ( 'NONE',  ( 0.1993543840281267465, 5.109805555631420582, 0.1993543840281266633 ) ) ;
#1900 = CARTESIAN_POINT ( 'NONE',  ( 1.995346317926969793E-07, 4.516063323326865664, 0.3119999999998666063 ) ) ;
#1901 = EDGE_LOOP ( 'NONE', ( #1640, #11283, #22607, #1928 ) ) ;
#1902 = CARTESIAN_POINT ( 'NONE',  ( -6.979263641208234666E-17, 0.04732142847388615819, 0.3799334167787516980 ) ) ;
#1903 = CARTESIAN_POINT ( 'NONE',  ( 0.04544327613271605115, 0.04227586460901846394, -0.2884427797219447087 ) ) ;
#1904 = APPROVAL_ROLE ( '' ) ;
#1905 = CARTESIAN_POINT ( 'NONE',  ( -3.863846776457871776E-17, -0.3155070326520292845, 0.4129861111111157168 ) ) ;
#1906 = CARTESIAN_POINT ( 'NONE',  ( -0.1993543840281266910, 5.068138888964754507, -0.1993543840281266910 ) ) ;
#1907 = CIRCLE ( 'NONE', #16711, 0.3125000000000000000 ) ;
#1908 = LINE ( 'NONE', #20208, #17736 ) ;
#1909 = LINE ( 'NONE', #16670, #18816 ) ;
#1910 = ORIENTED_EDGE ( 'NONE', *, *, #22477, .F. ) ;
#1911 = CARTESIAN_POINT ( 'NONE',  ( 0.2819296736111110979, 0.3270833332574666907, 0.000000000000000000 ) ) ;
#1912 = CARTESIAN_POINT ( 'NONE',  ( -0.1144950937579609918, -0.2764156081756484196, 0.3279166666666703533 ) ) ;
#1913 = EDGE_CURVE ( 'NONE', #6274, #11233, #22814, .T. ) ;
#1914 = CARTESIAN_POINT ( 'NONE',  ( 0.1167790944451422702, 4.904944444520311642, -0.2819296736111110424 ) ) ;
#1915 = CARTESIAN_POINT ( 'NONE',  ( 0.04944919563260133377, 5.072983550597543356, 0.3080590098858524417 ) ) ;
#1916 = ADVANCED_FACE ( 'NONE', ( #20983 ), #15148, .F. ) ;
#1917 = CARTESIAN_POINT ( 'NONE',  ( 0.1993543840281267465, 4.929250000075866112, 0.1993543840281266633 ) ) ;
#1918 = CARTESIAN_POINT ( 'NONE',  ( 0.000000000000000000, 5.384999999999999787, 0.000000000000000000 ) ) ;
#1919 = DIRECTION ( 'NONE',  ( 0.000000000000000000, 0.000000000000000000, -1.000000000000000000 ) ) ;
#1920 = DIRECTION ( 'NONE',  ( 0.000000000000000000, -1.000000000000000000, 0.000000000000000000 ) ) ;
#1921 = LINE ( 'NONE', #10960, #17040 ) ;
#1922 = CARTESIAN_POINT ( 'NONE',  ( -0.2206173157302028232, 4.543833333333332725, -0.2206173157302028232 ) ) ;
#1923 = DIRECTION ( 'NONE',  ( 0.7071067811865474617, 1.239037099348071290E-16, 0.7071067811865474617 ) ) ;
#1924 = CARTESIAN_POINT ( 'NONE',  ( 0.2673609140411699059, 4.025085253908718741, 0.1646236954874195357 ) ) ;
#1925 = CARTESIAN_POINT ( 'NONE',  ( -0.06562929165342790139, 3.736422086006603749, 0.3053604199167166411 ) ) ;
#1926 = AXIS2_PLACEMENT_3D ( 'NONE', #3996, #16814, #7891 ) ;
#1927 = SPHERICAL_SURFACE ( 'NONE', #1926, 0.01874999999999999931 ) ;
#1928 = ORIENTED_EDGE ( 'NONE', *, *, #3498, .F. ) ;
#1929 = CARTESIAN_POINT ( 'NONE',  ( -0.1491676245034612991, 4.122732337806922942, 0.2741778922001768537 ) ) ;
#1930 = CARTESIAN_POINT ( 'NONE',  ( 0.2764156081756484196, -5.077672346800151106E-17, 0.2827777777777812362 ) ) ;
#1931 = LINE ( 'NONE', #16820, #13848 ) ;
#1932 = CARTESIAN_POINT ( 'NONE',  ( -0.1917207807845848766, 4.454768623156928342, 0.2495099228813656700 ) ) ;
#1934 = VERTEX_POINT ( 'NONE', #625 ) ;
#1933 = CC_DESIGN_PERSON_AND_ORGANIZATION_ASSIGNMENT ( #6037, #5801, ( #582 ) ) ;
#1935 = AXIS2_PLACEMENT_3D ( 'NONE', #18041, #14031, #19753 ) ;
#1936 = CARTESIAN_POINT ( 'NONE',  ( 0.2233192592356399164, 0.2866071427596003640, 0.3073725909049500604 ) ) ;
#1937 = AXIS2_PLACEMENT_3D ( 'NONE', #23115, #19230, #4353 ) ;
#1938 = CARTESIAN_POINT ( 'NONE',  ( -0.2819296736111110424, 0.2819444443685777957, -0.1167790944451423396 ) ) ;
#1939 = CARTESIAN_POINT ( 'NONE',  ( 0.2495004542431085715, 3.869004524374595189, -0.1917331026496484903 ) ) ;
#1940 = CARTESIAN_POINT ( 'NONE',  ( 0.1579949080133604133, 0.7453945092721133703, -1.080137517429541782 ) ) ;
#1941 = CARTESIAN_POINT ( 'NONE',  ( -0.1294417382415922746, -0.3125000000000000000, 0.07097222222222378252 ) ) ;
#1942 = CARTESIAN_POINT ( 'NONE',  ( -0.1144950937579609918, -0.2764156081756484196, -0.06097222222222156013 ) ) ;
#1943 = VERTEX_POINT ( 'NONE', #8056 ) ;
#1944 = CARTESIAN_POINT ( 'NONE',  ( -1.906863420619159052E-17, 5.092106365077719410, -0.3114144293598434809 ) ) ;
#1945 = CARTESIAN_POINT ( 'NONE',  ( -0.2206173157302027676, 4.724388888888888083, 0.2206173157302028787 ) ) ;
#1946 = CARTESIAN_POINT ( 'NONE',  ( 0.1292346314604056745, 0.08402777777777743762, -0.3119999999999999996 ) ) ;
#1947 = CARTESIAN_POINT ( 'NONE',  ( 5.731347020009612645E-17, 5.064666666666665762, 0.3119999999999999996 ) ) ;
#1948 = CARTESIAN_POINT ( 'NONE',  ( 0.2233192592356399997, 0.3080357141881718275, -0.3073725909049500049 ) ) ;
#1949 = ORIENTED_EDGE ( 'NONE', *, *, #23147, .F. ) ;
#1950 = CARTESIAN_POINT ( 'NONE',  ( 5.178964085587577574E-17, 4.269527777853643791, 0.2819296736111110979 ) ) ;
#1951 = PRODUCT_DEFINITION_SHAPE ( 'NONE', 'NONE',  #24136 ) ;
#1952 = PLANE ( 'NONE',  #19774 ) ;
#1953 = CARTESIAN_POINT ( 'NONE',  ( 0.3473794045410782405, -4.100712535614411444E-18, -0.1022067409664305093 ) ) ;
#1954 = VERTEX_POINT ( 'NONE', #15504 ) ;
#1955 = ORIENTED_EDGE ( 'NONE', *, *, #7094, .F. ) ;
#1956 = CARTESIAN_POINT ( 'NONE',  ( 0.2712357692916257390, 4.358675636220367799, 0.1542604503148356232 ) ) ;
#1957 = CARTESIAN_POINT ( 'NONE',  ( -0.1993543840281266355, 4.970916666742532186, 0.1993543840281267465 ) ) ;
#1958 =( BOUNDED_CURVE ( )  B_SPLINE_CURVE ( 2, ( #3386, #12680, #1442, #8876, #12926, #16318, #1563, #22161, #11076 ),
 .UNSPECIFIED., .F., .F. ) 
 B_SPLINE_CURVE_WITH_KNOTS ( ( 3, 2, 2, 2, 3 ),
 ( 0.6458333333333333703, 0.6562500000000000000, 0.6666666666666667407, 0.6770833333333334814, 0.6875000000000001110 ),
 .UNSPECIFIED. ) 
 CURVE ( )  GEOMETRIC_REPRESENTATION_ITEM ( )  RATIONAL_B_SPLINE_CURVE ( ( 1.000000000000000000, 0.9238795325112867385, 1.000000000000000000, 0.9238795325112867385, 1.000000000000000000, 0.9238795325112867385, 1.000000000000000000, 0.9238795325112859613, 1.000000000000000888 ) ) 
 REPRESENTATION_ITEM ( '' )  );
#1959 = CARTESIAN_POINT ( 'NONE',  ( 0.008702674981888494643, 5.198088336626264017, 0.2858269518860258041 ) ) ;
#1960 = CIRCLE ( 'NONE', #11316, 0.4625000000000000777 ) ;
#1961 = ADVANCED_FACE ( 'NONE', ( #22931 ), #20624, .T. ) ;
#1962 = DIRECTION ( 'NONE',  ( 0.000000000000000000, 0.000000000000000000, 1.000000000000000000 ) ) ;
#1963 = VECTOR ( 'NONE', #18895, 39.37007874015748143 ) ;
#1964 = DIRECTION ( 'NONE',  ( 0.000000000000000000, 0.000000000000000000, 1.000000000000000000 ) ) ;
#1965 = CARTESIAN_POINT ( 'NONE',  ( 0.07134304080793986425, 3.708532704952418602, -0.3042648351956888098 ) ) ;
#1966 = CARTESIAN_POINT ( 'NONE',  ( 0.3999999999999999667, 0.1892857142857141961, -0.1299678784931625197 ) ) ;
#1967 = CARTESIAN_POINT ( 'NONE',  ( 0.2819296736111110979, 4.717444444520309865, -0.1167790944451423396 ) ) ;
#1968 = ITEM_DEFINED_TRANSFORMATION ( 'NONE', 'NONE', #19639,  #9127 ) ;
#1969 = CC_DESIGN_PERSON_AND_ORGANIZATION_ASSIGNMENT ( #519, #22715, ( #10911 ) ) ;
#1970 = CARTESIAN_POINT ( 'NONE',  ( 2.170194434256479177, 2.290013683160381674, -2.965986316839620773 ) ) ;
#1971 = DIRECTION ( 'NONE',  ( -0.4985709748471498504, -0.07555085810113110201, -0.8635502596144276621 ) ) ;
#1972 = CARTESIAN_POINT ( 'NONE',  ( -0.2819296736111110979, 0.5805555554796888451, 0.1167790944451422425 ) ) ;
#1973 = EDGE_LOOP ( 'NONE', ( #14961, #7082 ) ) ;
#1974 = ORIENTED_EDGE ( 'NONE', *, *, #2134, .F. ) ;
#1975 = CARTESIAN_POINT ( 'NONE',  ( -0.1993543840281267465, 0.2506944443685777957, 0.1993543840281266633 ) ) ;
#1976 = FACE_OUTER_BOUND ( 'NONE', #16823, .T. ) ;
#1977 = DIRECTION ( 'NONE',  ( -0.000000000000000000, -1.000000000000000000, -0.000000000000000000 ) ) ;
#1978 = CARTESIAN_POINT ( 'NONE',  ( -0.4000000000000000222, 0.2964285714285713191, 0.1299678784931624920 ) ) ;
#1979 = CARTESIAN_POINT ( 'NONE',  ( 0.2230971623002954429, 0.2230971623002953319, 0.04145833333333462378 ) ) ;
#1980 = CARTESIAN_POINT ( 'NONE',  ( 0.4687500000000002220, -0.08766214734763430605, 0.4143508694870877695 ) ) ;
#1981 = VECTOR ( 'NONE', #8238, 39.37007874015748854 ) ;
#1982 = DIRECTION ( 'NONE',  ( -0.000000000000000000, -0.000000000000000000, -1.000000000000000000 ) ) ;
#1983 = CARTESIAN_POINT ( 'NONE',  ( -0.2819296736111111534, 0.2888888888130223265, 0.1167790944451422563 ) ) ;
#1984 = CARTESIAN_POINT ( 'NONE',  ( -0.1993543840281266633, 0.05624999992413336897, -0.1993543840281266910 ) ) ;
#1985 = AXIS2_PLACEMENT_3D ( 'NONE', #8316, #6979, #21848 ) ;
#1986 = CARTESIAN_POINT ( 'NONE',  ( 0.1167790944451422702, 4.238277777853643791, -0.2819296736111110424 ) ) ;
#1987 = CARTESIAN_POINT ( 'NONE',  ( -0.4000000000000000222, 0.1410714283763437882, -4.898587196589413075E-17 ) ) ;
#1988 = CARTESIAN_POINT ( 'NONE',  ( -0.1167790944451423257, 5.078555555631421470, -0.2819296736111110424 ) ) ;
#1989 = CARTESIAN_POINT ( 'NONE',  ( 0.1993543840281267465, 4.484805555631420582, 0.1993543840281266633 ) ) ;
#1990 = CARTESIAN_POINT ( 'NONE',  ( 0.3214243565000137748, 2.693118229757915039, -1.028079841261090754 ) ) ;
#1991 = ORIENTED_EDGE ( 'NONE', *, *, #22138, .F. ) ;
#1992 = CARTESIAN_POINT ( 'NONE',  ( -0.2725578398252894718, 0.3839045351724006960, 0.09139393128959945323 ) ) ;
#1993 = CARTESIAN_POINT ( 'NONE',  ( 0.2206173157302028787, 4.078555555707287894, 0.2206173157302027954 ) ) ;
#1994 = CARTESIAN_POINT ( 'NONE',  ( -0.4225900379021583775, 0.2972834052256090320, 0.3902123106865083568 ) ) ;
#1995 = LENGTH_MEASURE_WITH_UNIT ( LENGTH_MEASURE( 0.02539999999999999897 ), #19058 );
#1996 = EDGE_LOOP ( 'NONE', ( #8675, #6494, #19229, #22769 ) ) ;
#1997 = TOROIDAL_SURFACE ( 'NONE', #13311, 0.2510000000000000009, 0.001000000000000037101 ) ;
#1998 = ORIENTED_EDGE ( 'NONE', *, *, #124, .F. ) ;
#1999 = PERSON_AND_ORGANIZATION_ROLE ( 'design_supplier' ) ;
#2000 = CARTESIAN_POINT ( 'NONE',  ( -0.2256529556066708964, -0.2011140187169780102, 0.4134710460457109438 ) ) ;
#2001 = EDGE_CURVE ( 'NONE', #20538, #3958, #8171, .T. ) ;
#2002 = CARTESIAN_POINT ( 'NONE',  ( -0.1383363854359150602, 4.845312163550097750, 0.2796553313559969056 ) ) ;
#2003 = CARTESIAN_POINT ( 'NONE',  ( 0.000000000000000000, 0.000000000000000000, 1.223000000000000309 ) ) ;
#2004 = VERTEX_POINT ( 'NONE', #2695 ) ;
#2005 = CARTESIAN_POINT ( 'NONE',  ( -0.1292346314604058410, 0.4381944442927114824, 0.3119999999999998885 ) ) ;
#2006 = ORIENTED_EDGE ( 'NONE', *, *, #15547, .F. ) ;
#2007 = CARTESIAN_POINT ( 'NONE',  ( 0.3125000000000000000, 3.827021247335477694E-17, 1.326383476483184332 ) ) ;
#2008 = CARTESIAN_POINT ( 'NONE',  ( 0.1683412523880292166, 4.743237864158165173, 0.2653294386633363033 ) ) ;
#2009 = CARTESIAN_POINT ( 'NONE',  ( -6.979263641208234666E-17, 0.1187499999024575897, 0.3799334167787516425 ) ) ;
#2010 = CARTESIAN_POINT ( 'NONE',  ( 0.08174464492498181856, 3.985945071896700664, -0.3038634887636957882 ) ) ;
#2011 =( BOUNDED_SURFACE ( )  B_SPLINE_SURFACE ( 3, 2, ( 
 ( #12039, #8471, #2996 ),
 ( #14092, #16043, #23457 ),
 ( #23097, #10323, #15911 ),
 ( #21519, #4810, #8713 ),
 ( #13974, #6767, #14212 ),
 ( #6526, #21646, #4935 ),
 ( #6406, #16162, #4454 ),
 ( #12400, #3114, #10562 ),
 ( #917, #6286, #19338 ),
 ( #2634, #10083, #4580 ),
 ( #15679, #19453, #2751 ),
 ( #10202, #1884, #18350 ) ),
 .UNSPECIFIED., .F., .F., .F. ) 
 B_SPLINE_SURFACE_WITH_KNOTS ( ( 4, 2, 2, 2, 2, 4 ),
 ( 3, 3 ),
 ( 0.02197974498297192159, 0.02532345735115096308, 0.02699531353524048383, 0.02866716971933000457, 0.03201088208750904607, 0.03535459445568808756 ),
 ( 0.000000000000000000, 1.000000000000000000 ),
 .UNSPECIFIED. ) 
 GEOMETRIC_REPRESENTATION_ITEM ( )  RATIONAL_B_SPLINE_SURFACE ( (
 ( 1.000000000000000000, 0.8464669816041905381, 1.000000000000000000),
 ( 1.000000000000000000, 0.8516228929821839655, 1.000000000000000000),
 ( 1.000000000000000000, 0.8565470209672587654, 1.000000000000000000),
 ( 1.000000000000000000, 0.8619809739981544316, 1.000000000000000000),
 ( 1.000000000000000000, 0.8634611050169099800, 1.000000000000000000),
 ( 1.000000000000000000, 0.8654882157366866613, 1.000000000000000000),
 ( 1.000000000000000000, 0.8660234405451954220, 1.000000000000000000),
 ( 1.000000000000000000, 0.8660293137690006082, 1.000000000000000000),
 ( 1.000000000000000000, 0.8638069272854496106, 1.000000000000000000),
 ( 1.000000000000000000, 0.8565545265013099208, 1.000000000000000000),
 ( 1.000000000000000000, 0.8516246201512510661, 1.000000000000000000),
 ( 1.000000000000000000, 0.8464669816041905381, 1.000000000000000000) ) ) 
 REPRESENTATION_ITEM ( '' )  SURFACE ( )  );
#2012 = ORIENTED_EDGE ( 'NONE', *, *, #20943, .F. ) ;
#2013 = CARTESIAN_POINT ( 'NONE',  ( 0.1116596296178199027, 0.06874999990245758696, 0.3436530038418508792 ) ) ;
#2014 = VERTEX_POINT ( 'NONE', #1102 ) ;
#2015 = CARTESIAN_POINT ( 'NONE',  ( 0.000000000000000000, 0.000000000000000000, 0.000000000000000000 ) ) ;
#2016 = CARTESIAN_POINT ( 'NONE',  ( -0.3058739907781938272, 4.667087298452083921, -0.06261323344678072778 ) ) ;
#2017 = CARTESIAN_POINT ( 'NONE',  ( 0.1993543840281267465, 4.207027777853643791, 0.1993543840281266633 ) ) ;
#2018 = CARTESIAN_POINT ( 'NONE',  ( 0.1689451345729078013, -0.2321341939677896704, 0.3986378631856341004 ) ) ;
#2019 = CARTESIAN_POINT ( 'NONE',  ( 0.000000000000000000, 0.1199999999999999956, -0.3150000000000000022 ) ) ;
#2020 = CARTESIAN_POINT ( 'NONE',  ( 0.2206173157302027954, 3.807722222222221564, -0.2206173157302028232 ) ) ;
#2021 = CARTESIAN_POINT ( 'NONE',  ( -0.2206173157302027676, 4.731333333485065573, 0.2206173157302028787 ) ) ;
#2022 = CARTESIAN_POINT ( 'NONE',  ( 0.3091789633153798067, 4.806552312893038525, 0.04229410102701547380 ) ) ;
#2023 = EDGE_CURVE ( 'NONE', #11875, #11539, #20335, .T. ) ;
#2024 = CARTESIAN_POINT ( 'NONE',  ( -2.336494862270849996E-07, 3.904935224540334815, 0.3119999999998144258 ) ) ;
#2025 = CARTESIAN_POINT ( 'NONE',  ( -0.2233192592356399442, 0.2330357141881718719, -0.3073725909049499494 ) ) ;
#2026 = CARTESIAN_POINT ( 'NONE',  ( 0.2787925280157932950, 0.03555950194956544741, -0.06367239110606161268 ) ) ;
#2027 = ORIENTED_EDGE ( 'NONE', *, *, #16781, .F. ) ;
#2028 = B_SPLINE_CURVE_WITH_KNOTS ( 'NONE', 3,
 ( #6209, #22674, #3452, #20848, #28, #2441, #11713, #12990, #11595, #7803, #9884, #12868 ),
 .UNSPECIFIED., .F., .F.,
 ( 4, 2, 2, 2, 2, 4 ),
 ( 0.000000000000000000, 0.003384026746073582302, 0.006768053492147164604, 0.008460066865183954454, 0.01015208023822074777, 0.01353610698429432574 ),
 .UNSPECIFIED. ) ;
#2029 = CALENDAR_DATE ( 2026, 7, 10 ) ;
#2030 = EDGE_CURVE ( 'NONE', #21724, #2478, #12342, .T. ) ;
#2031 = CARTESIAN_POINT ( 'NONE',  ( 0.2230971623002954429, 0.2230971623002953319, 0.4338194444444492537 ) ) ;
#2032 = CARTESIAN_POINT ( 'NONE',  ( 0.1993543840281266633, 5.109805555631420582, -0.1993543840281266910 ) ) ;
#2033 = CARTESIAN_POINT ( 'NONE',  ( 0.2819296736111110979, 3.838972222298087544, -3.452642723725051716E-17 ) ) ;
#2034 = LINE ( 'NONE', #9471, #14651 ) ;
#2035 = DIRECTION ( 'NONE',  ( -0.000000000000000000, -1.000000000000000000, -0.000000000000000000 ) ) ;
#2036 = CARTESIAN_POINT ( 'NONE',  ( -3.385114897866767815E-17, -0.2764156081756484196, 0.1022222222222241989 ) ) ;
#2037 = CARTESIAN_POINT ( 'NONE',  ( 1.726321361862525858E-17, 0.3965277777019111105, -0.2819296736111110979 ) ) ;
#2038 = CARTESIAN_POINT ( 'NONE',  ( -3.385114897866767815E-17, -0.2764156081756484196, 0.3869444444444486431 ) ) ;
#2039 = CARTESIAN_POINT ( 'NONE',  ( 5.178964085587577574E-17, 5.047305555631421470, 0.2819296736111110979 ) ) ;
#2040 = CARTESIAN_POINT ( 'NONE',  ( -0.1236067977499789583, 0.4124999998049150851, -0.3804226065180614791 ) ) ;
#2041 = AXIS2_PLACEMENT_3D ( 'NONE', #15572, #9607, #22995 ) ;
#2042 = CARTESIAN_POINT ( 'NONE',  ( -0.1993543840281266355, 4.804250000075865223, 0.1993543840281267465 ) ) ;
#2043 = CARTESIAN_POINT ( 'NONE',  ( -0.02036395251267785617, 4.182136029502010466, 0.3120000006060605902 ) ) ;
#2044 = CARTESIAN_POINT ( 'NONE',  ( -0.2206173157302028232, 5.043833333333332725, -0.2206173157302028232 ) ) ;
#2045 = DIRECTION ( 'NONE',  ( 0.000000000000000000, 0.9659258262890680902, 0.2588190451025215166 ) ) ;
#2046 = DIRECTION ( 'NONE',  ( 0.8660254037844382635, 0.000000000000000000, 0.5000000000000005551 ) ) ;
#2047 = CARTESIAN_POINT ( 'NONE',  ( -0.3119999999999998885, 4.554249999999999687, 0.1292346314604058410 ) ) ;
#2048 = CARTESIAN_POINT ( 'NONE',  ( -0.2819296736111110979, 3.738277777853643791, -0.1167790944451422980 ) ) ;
#2049 = CARTESIAN_POINT ( 'NONE',  ( -0.3119999999999999996, 4.217444444444443441, 0.000000000000000000 ) ) ;
#2050 = CARTESIAN_POINT ( 'NONE',  ( 0.001511429766296307989, 4.988234430213637438, -0.3119965677994301356 ) ) ;
#2051 = CARTESIAN_POINT ( 'NONE',  ( -0.1036374797578168139, 3.735295676787865116, 0.2942854964279391639 ) ) ;
#2052 = CARTESIAN_POINT ( 'NONE',  ( -0.6398935782932173577, 0.000000000000000000, -0.1019043464467004889 ) ) ;
#2053 = VERTEX_POINT ( 'NONE', #12222 ) ;
#2054 = DIRECTION ( 'NONE',  ( 0.000000000000000000, 0.000000000000000000, -1.000000000000000000 ) ) ;
#2055 = EDGE_CURVE ( 'NONE', #19443, #11353, #12456, .T. ) ;
#2056 = CIRCLE ( 'NONE', #9460, 0.6396424860381280109 ) ;
#2057 = CARTESIAN_POINT ( 'NONE',  ( 0.1144950937579609085, -0.2764156081756484751, 0.4390277777777825130 ) ) ;
#2058 = DIRECTION ( 'NONE',  ( 0.000000000000000000, 0.000000000000000000, 1.000000000000000000 ) ) ;
#2059 = ORIENTED_EDGE ( 'NONE', *, *, #21038, .F. ) ;
#2060 = CARTESIAN_POINT ( 'NONE',  ( -0.3613381517857144343, 0.1937499999024575870, 0.1174058825155740171 ) ) ;
#2061 = CARTESIAN_POINT ( 'NONE',  ( -0.1167790944451424368, 0.4069444443685779067, 0.2819296736111110424 ) ) ;
#2062 = CARTESIAN_POINT ( 'NONE',  ( 0.2726200149141687623, 3.858738252036598482, 0.1571313599304320630 ) ) ;
#2063 = CARTESIAN_POINT ( 'NONE',  ( 0.2371649040148513243, 0.6790977978122471059, -1.083707372304768324 ) ) ;
#2064 = LINE ( 'NONE', #5248, #23992 ) ;
#2065 = DIRECTION ( 'NONE',  ( -1.224646799147353207E-16, 0.000000000000000000, -1.000000000000000000 ) ) ;
#2066 = CARTESIAN_POINT ( 'NONE',  ( -0.2764156081756484196, 0.1144950937579609918, 0.2029166666666694097 ) ) ;
#2067 = CARTESIAN_POINT ( 'NONE',  ( -0.3385998376278290256, 3.738758431839877614E-19, -0.1012499999999999928 ) ) ;
#2068 = FACE_OUTER_BOUND ( 'NONE', #162, .T. ) ;
#2069 = CARTESIAN_POINT ( 'NONE',  ( -0.2206173157302028787, 0.3305555555555552139, 0.2206173157302027954 ) ) ;
#2070 = CARTESIAN_POINT ( 'NONE',  ( 0.3119999999999999996, 5.248694444444444329, -0.1292346314604056745 ) ) ;
#2071 = VECTOR ( 'NONE', #22271, 39.37007874015748143 ) ;
#2072 = CARTESIAN_POINT ( 'NONE',  ( 0.2819296736111110424, 4.120222222298087544, -0.1167790944451423396 ) ) ;
#2073 = FACE_OUTER_BOUND ( 'NONE', #4142, .T. ) ;
#2074 = LINE ( 'NONE', #7915, #19209 ) ;
#2075 = B_SPLINE_CURVE_WITH_KNOTS ( 'NONE', 3,
 ( #21997, #18105, #23812, #1638, #14456, #20177, #18344, #7254, #23939, #5046, #8956, #3344, #7134, #12759, #14574, #7370, #12516, #14820 ),
 .UNSPECIFIED., .F., .F.,
 ( 4, 2, 2, 2, 2, 2, 2, 2, 4 ),
 ( 0.1736046203853397751, 0.1758900224122931233, 0.1781754244392464714, 0.1804608264661998196, 0.1827462284931531677, 0.1850316305201065159, 0.1873170325470598641, 0.1896024345740132122, 0.1918878366009665604 ),
 .UNSPECIFIED. ) ;
#2076 = ORIENTED_EDGE ( 'NONE', *, *, #8881, .T. ) ;
#2077 = EDGE_LOOP ( 'NONE', ( #709, #23821, #14936, #3516 ) ) ;
#2078 = CARTESIAN_POINT ( 'NONE',  ( -0.4673607484394256550, -0.2845795129072106744, 0.04287645741408788874 ) ) ;
#2079 = CARTESIAN_POINT ( 'NONE',  ( -0.2819296736111110979, 4.908416666742532186, 0.000000000000000000 ) ) ;
#2080 = CARTESIAN_POINT ( 'NONE',  ( -1.861236469537744314E-17, 5.143359825938298435, -0.3039629827691722741 ) ) ;
#2081 = EDGE_CURVE ( 'NONE', #4938, #5470, #15859, .T. ) ;
#2082 = CARTESIAN_POINT ( 'NONE',  ( 0.4796770407326167995, -0.08628433980660102365, 0.07157439050488961785 ) ) ;
#2083 = DIRECTION ( 'NONE',  ( 0.000000000000000000, 0.000000000000000000, -1.000000000000000000 ) ) ;
#2084 = CARTESIAN_POINT ( 'NONE',  ( -0.1167790944451423535, 4.641055555631421470, 0.2819296736111110979 ) ) ;
#2085 = CONICAL_SURFACE ( 'NONE', #2849, 0.7500000000000001110, 0.7853981633974482790 ) ;
#2086 = CARTESIAN_POINT ( 'NONE',  ( -0.004140126504927462738, 4.043944831220694702, -0.3119764910025323856 ) ) ;
#2087 = CARTESIAN_POINT ( 'NONE',  ( -0.1954553509668046640, 0.1954553509668046918, 0.08833333333333517889 ) ) ;
#2088 = CARTESIAN_POINT ( 'NONE',  ( 0.1167790944451423535, 0.5388888888130223265, 0.2819296736111110424 ) ) ;
#2089 = EDGE_LOOP ( 'NONE', ( #8680, #3703, #7199, #248 ) ) ;
#2090 = CARTESIAN_POINT ( 'NONE',  ( 0.2819296736111110424, 0.3305555554796888451, -0.1167790944451423119 ) ) ;
#2091 = CARTESIAN_POINT ( 'NONE',  ( 1.910449006669871087E-17, 0.3583333331816003775, -0.3119999999999999996 ) ) ;
#2092 = CARTESIAN_POINT ( 'NONE',  ( 0.3125000000000004996, -0.1294417382415918583, 0.1959722222222248234 ) ) ;
#2093 = CARTESIAN_POINT ( 'NONE',  ( 0.3236067977499790249, 0.1214285714285713996, -0.2351141009169892826 ) ) ;
#2094 = CARTESIAN_POINT ( 'NONE',  ( 0.1306872919485614071, -0.3155070326520293955, -0.08701388888888861306 ) ) ;
#2095 = CARTESIAN_POINT ( 'NONE',  ( 0.4687500000000002220, -0.1526433126687117836, 0.4038658439110331955 ) ) ;
#2096 = ADVANCED_FACE ( 'NONE', ( #3167 ), #18047, .T. ) ;
#2097 = CARTESIAN_POINT ( 'NONE',  ( -1.910449006669871087E-17, 5.036888888888888971, -0.3119999999999999996 ) ) ;
#2098 = CARTESIAN_POINT ( 'NONE',  ( 1.726321361862525858E-17, 0.2159722221463555858, -0.2819296736111110979 ) ) ;
#2099 = CARTESIAN_POINT ( 'NONE',  ( 0.1993543840281266355, 0.1951388888130222155, 0.1993543840281267465 ) ) ;
#2100 = CARTESIAN_POINT ( 'NONE',  ( -1.726321361862525858E-17, 4.297305555631421470, -0.2819296736111110979 ) ) ;
#2101 = CARTESIAN_POINT ( 'NONE',  ( 0.2472135954999579166, 0.02321428551920093342, 0.3402603233408160732 ) ) ;
#2102 = EDGE_CURVE ( 'NONE', #18764, #6009, #9115, .T. ) ;
#2103 = CARTESIAN_POINT ( 'NONE',  ( -0.1167790944451423257, 4.911888888964755395, -0.2819296736111110424 ) ) ;
#2104 = CARTESIAN_POINT ( 'NONE',  ( -0.2819296736111110424, 4.467444444520309865, 0.1167790944451424923 ) ) ;
#2105 = DIRECTION ( 'NONE',  ( 0.000000000000000000, 0.000000000000000000, -1.000000000000000000 ) ) ;
#2106 = ORIENTED_EDGE ( 'NONE', *, *, #8432, .F. ) ;
#2107 = CARTESIAN_POINT ( 'NONE',  ( 0.1294417382415921358, -0.3125000000000002220, 0.2445833333333362336 ) ) ;
#2108 = CC_DESIGN_PERSON_AND_ORGANIZATION_ASSIGNMENT ( #8403, #23392, ( #1033 ) ) ;
#2109 = CARTESIAN_POINT ( 'NONE',  ( 0.3119999999999999996, 3.977861111262842808, -0.1292346314604056745 ) ) ;
#2110 = CIRCLE ( 'NONE', #18838, 0.4000000000000000222 ) ;
#2111 = CARTESIAN_POINT ( 'NONE',  ( -9.626299801968715084E-16, 0.2660714283763437327, -0.4000000000000000222 ) ) ;
#2112 = CARTESIAN_POINT ( 'NONE',  ( -0.09493784612928136968, -0.2937490000082879082, -0.09741978624864720826 ) ) ;
#2113 = ORIENTED_EDGE ( 'NONE', *, *, #9831, .T. ) ;
#2114 = DATE_AND_TIME ( #7839, #14636 ) ;
#2115 = ORIENTED_EDGE ( 'NONE', *, *, #20324, .F. ) ;
#2116 = CARTESIAN_POINT ( 'NONE',  ( 7.515426412127797749E-07, 4.849418923572540230, 0.3119999999980542227 ) ) ;
#2117 = CARTESIAN_POINT ( 'NONE',  ( -0.2722822261173367120, 4.997487659248541547, -0.1577061459665719811 ) ) ;
#2118 = VERTEX_POINT ( 'NONE', #13799 ) ;
#2119 = B_SPLINE_CURVE_WITH_KNOTS ( 'NONE', 3,
 ( #4000, #15110, #7783, #5586, #18758, #5471, #1929, #14989, #5828, #20347, #24113, #7305, #18884, #9251, #22658, #14875, #20469, #13052, #5946, #2184, #9374, #9128, #20231, #3520, #10971, #11328, #16928, #3637, #3768, #7660, #13291, #16815, #7541, #18395 ),
 .UNSPECIFIED., .F., .F.,
 ( 4, 2, 2, 2, 1, 1, 1, 2, 2, 1, 2, 2, 2, 2, 2, 2, 2, 2, 4 ),
 ( 0.7232422263945339491, 0.7242982534508761727, 0.7248262669790472845, 0.7250902737431328404, 0.7252222771251756184, 0.7252552779706863406, 0.7252717783934417017, 0.7252759034991305143, 0.7252800286048193268, 0.7252882788161969518, 0.7253542805072183963, 0.7274663346199028435, 0.7295783887325872907, 0.7316904428452717379, 0.7327464699016139615, 0.7338024969579561851, 0.7359145510706406323, 0.7380266051833250796, 0.7401386592960095268 ),
 .UNSPECIFIED. ) ;
#2120 = CARTESIAN_POINT ( 'NONE',  ( -0.3119999999999999996, 0.5909722220704892726, -0.1292346314604056745 ) ) ;
#2121 = EDGE_LOOP ( 'NONE', ( #8010, #18293, #8192, #17141, #8307, #11387, #13181, #23760, #1870, #434 ) ) ;
#2122 = CARTESIAN_POINT ( 'NONE',  ( 0.7847114317029997288, 2.978485840173427324, -0.8855837454876586134 ) ) ;
#2123 = CARTESIAN_POINT ( 'NONE',  ( -1.910449006669871087E-17, 4.481333333333331836, -0.3119999999999999996 ) ) ;
#2124 = DIRECTION ( 'NONE',  ( 0.000000000000000000, 0.000000000000000000, 1.000000000000000000 ) ) ;
#2125 = VECTOR ( 'NONE', #12994, 39.37007874015747433 ) ;
#2126 = CARTESIAN_POINT ( 'NONE',  ( -0.3613381517857143232, 0.09732142847388615403, -0.1174058825155741004 ) ) ;
#2127 = CARTESIAN_POINT ( 'NONE',  ( 0.2493652384627738638, 3.968578555994963786, 0.1919023481737216208 ) ) ;
#2128 = ORIENTED_EDGE ( 'NONE', *, *, #6335, .F. ) ;
#2129 = EDGE_CURVE ( 'NONE', #15581, #20003, #1264, .T. ) ;
#2130 = CARTESIAN_POINT ( 'NONE',  ( 0.2233192592356399164, 0.2151785713310289949, 0.3073725909049500604 ) ) ;
#2131 = ORIENTED_EDGE ( 'NONE', *, *, #21045, .F. ) ;
#2132 = CARTESIAN_POINT ( 'NONE',  ( 0.000000000000000000, 3.659999999999999698, 0.000000000000000000 ) ) ;
#2133 = CARTESIAN_POINT ( 'NONE',  ( -0.2901014048727216799, 4.672287041779367378, 0.1163490317311436512 ) ) ;
#2134 = EDGE_CURVE ( 'NONE', #14350, #20423, #5074, .T. ) ;
#2135 = CARTESIAN_POINT ( 'NONE',  ( -0.2819296736111110979, 3.908416666742532630, 0.000000000000000000 ) ) ;
#2136 = CARTESIAN_POINT ( 'NONE',  ( 0.1675091558324258156, 5.038924456986563882, -0.2640337788857253787 ) ) ;
#2137 = CARTESIAN_POINT ( 'NONE',  ( -0.3119999999999999996, 4.825083333333331836, -0.1292346314604056468 ) ) ;
#2138 =( GEOMETRIC_REPRESENTATION_CONTEXT ( 3 ) GLOBAL_UNCERTAINTY_ASSIGNED_CONTEXT ( ( #17531 ) ) GLOBAL_UNIT_ASSIGNED_CONTEXT ( ( #20141, #6852, #16366 ) ) REPRESENTATION_CONTEXT ( 'NONE', 'WORKASPACE' ) );
#2139 = CARTESIAN_POINT ( 'NONE',  ( -0.2206173157302028232, 3.877166666666666206, -0.2206173157302028232 ) ) ;
#2140 = CARTESIAN_POINT ( 'NONE',  ( 2.319244702705235195, 2.291712385858714729, -2.476240473580834323 ) ) ;
#2141 = CARTESIAN_POINT ( 'NONE',  ( -0.1292346314604057023, 4.679250000151732536, 0.3119999999999998885 ) ) ;
#2142 = EDGE_CURVE ( 'NONE', #12951, #404, #11183, .T. ) ;
#2143 = CARTESIAN_POINT ( 'NONE',  ( -0.2819296736111110979, 5.033416666742532186, 0.000000000000000000 ) ) ;
#2144 = ORIENTED_EDGE ( 'NONE', *, *, #12577, .T. ) ;
#2145 = CARTESIAN_POINT ( 'NONE',  ( 0.1993543840281266633, 4.387583333409199149, -0.1993543840281266910 ) ) ;
#2146 = CARTESIAN_POINT ( 'NONE',  ( -0.2229596387321840234, 3.897916385485626911, 0.2198564724305951679 ) ) ;
#2147 = ORIENTED_EDGE ( 'NONE', *, *, #22390, .F. ) ;
#2148 = CARTESIAN_POINT ( 'NONE',  ( -0.2233192592356400275, 0.1116071427596004445, 0.3073725909049499494 ) ) ;
#2149 = VECTOR ( 'NONE', #3040, 39.37007874015748854 ) ;
#2150 = ORIENTED_EDGE ( 'NONE', *, *, #16482, .T. ) ;
#2151 = ORIENTED_EDGE ( 'NONE', *, *, #1913, .T. ) ;
#2152 = COORDINATED_UNIVERSAL_TIME_OFFSET ( 0, 0, .AHEAD. ) ;
#2153 = ORIENTED_EDGE ( 'NONE', *, *, #17718, .T. ) ;
#2154 =( BOUNDED_CURVE ( )  B_SPLINE_CURVE ( 2, ( #4765, #6723, #21596, #23529, #6363, #17584, #6482, #13703, #11874 ),
 .UNSPECIFIED., .F., .T. ) 
 B_SPLINE_CURVE_WITH_KNOTS ( ( 3, 2, 2, 2, 3 ),
 ( 0.5625000000000000000, 0.5729166666666666297, 0.5833333333333333703, 0.5937500000000000000, 0.6041666666666666297 ),
 .UNSPECIFIED. ) 
 CURVE ( )  GEOMETRIC_REPRESENTATION_ITEM ( )  RATIONAL_B_SPLINE_CURVE ( ( 1.000000000000000000, 0.9238795325112867385, 1.000000000000000000, 0.9238795325112867385, 1.000000000000000000, 0.9238795325112867385, 1.000000000000000000, 0.9238795325112867385, 1.000000000000000000 ) ) 
 REPRESENTATION_ITEM ( '' )  );
#2155 = CARTESIAN_POINT ( 'NONE',  ( 0.2230971623002954429, 0.2230971623002953319, 0.3782638888888932849 ) ) ;
#2156 = CARTESIAN_POINT ( 'NONE',  ( 0.2819296736111110979, 5.099388888964754507, 0.1167790944451422425 ) ) ;
#2157 =( BOUNDED_SURFACE ( )  B_SPLINE_SURFACE ( 3, 2, ( 
 ( #20225, #1803, #12560 ),
 ( #9120, #23622, #20343 ),
 ( #3515, #18390, #23736 ),
 ( #7060, #14373, #10965 ),
 ( #1685, #16568, #3631 ),
 ( #14499, #23990, #14751 ) ),
 .UNSPECIFIED., .F., .F., .T. ) 
 B_SPLINE_SURFACE_WITH_KNOTS ( ( 4, 2, 4 ),
 ( 3, 3 ),
 ( 0.001790663949227914217, 0.002289857484343688597, 0.002789051019459462544 ),
 ( 0.000000000000000000, 1.000000000000000000 ),
 .UNSPECIFIED. ) 
 GEOMETRIC_REPRESENTATION_ITEM ( )  RATIONAL_B_SPLINE_SURFACE ( (
 ( 1.000000000000000000, 0.8285407536241355952, 1.000000000000000000),
 ( 1.000000000000000000, 0.8382697314792758592, 1.000000000000000000),
 ( 1.000000000000000000, 0.8433836253083885071, 1.000000000000000000),
 ( 1.000000000000000000, 0.8433992480894890731, 1.000000000000000000),
 ( 1.000000000000000000, 0.8382827608169696187, 1.000000000000000000),
 ( 1.000000000000000000, 0.8285407536241035098, 1.000000000000000000) ) ) 
 REPRESENTATION_ITEM ( '' )  SURFACE ( )  );
#2158 = APPROVAL_PERSON_ORGANIZATION ( #12446, #19972, #1904 ) ;
#2159 = CARTESIAN_POINT ( 'NONE',  ( 0.1993543840281267465, 3.887583333409199149, 0.1993543840281266633 ) ) ;
#2160 = DIRECTION ( 'NONE',  ( -0.000000000000000000, -1.000000000000000000, -0.000000000000000000 ) ) ;
#2161 = CARTESIAN_POINT ( 'NONE',  ( -0.2206173157302027676, 4.946611111111110404, 0.2206173157302028787 ) ) ;
#2162 = ADVANCED_FACE ( 'NONE', ( #16101 ), #23515, .T. ) ;
#2163 = EDGE_CURVE ( 'NONE', #14885, #20299, #4639, .T. ) ;
#2164 = CARTESIAN_POINT ( 'NONE',  ( 0.2764156081756483641, -0.1144950937579611028, 0.3348611111111149952 ) ) ;
#2165 = CARTESIAN_POINT ( 'NONE',  ( -0.2819296736111111534, 0.4694444443685776847, 0.1167790944451422563 ) ) ;
#2166 = CARTESIAN_POINT ( 'NONE',  ( 0.1144950937579609085, -0.2764156081756484751, -0.06097222222222153931 ) ) ;
#2167 = CARTESIAN_POINT ( 'NONE',  ( 0.1167790944451422702, 4.849388888964755395, -0.2819296736111110424 ) ) ;
#2168 = FACE_OUTER_BOUND ( 'NONE', #14401, .T. ) ;
#2169 = CONICAL_SURFACE ( 'NONE', #10726, 0.3125000000000000000, 0.7853981633974497223 ) ;
#2170 = CARTESIAN_POINT ( 'NONE',  ( -0.2819296736111110424, 4.578555555631421470, 0.1167790944451424923 ) ) ;
#2171 = CARTESIAN_POINT ( 'NONE',  ( -0.2784250239278213690, 0.03789337644375285336, -0.06999960198848567683 ) ) ;
#2172 = CARTESIAN_POINT ( 'NONE',  ( 0.2874075015922078480, 4.866815774503709946, -0.1215004182914477260 ) ) ;
#2173 = DIRECTION ( 'NONE',  ( 0.7745966692414850696, -0.4472135954999565954, 0.4472135954999565954 ) ) ;
#2174 = LINE ( 'NONE', #13282, #20158 ) ;
#2175 = CARTESIAN_POINT ( 'NONE',  ( 5.731347020009612645E-17, 4.564666666666665762, 0.3119999999999999996 ) ) ;
#2176 = CARTESIAN_POINT ( 'NONE',  ( -0.1167790944451423119, 3.842444444520309865, -0.2819296736111110979 ) ) ;
#2177 = FACE_OUTER_BOUND ( 'NONE', #10912, .T. ) ;
#2178 = EDGE_CURVE ( 'NONE', #23965, #1058, #6891, .T. ) ;
#2179 = CARTESIAN_POINT ( 'NONE',  ( 0.02106080771364779100, 4.987673659226542711, -0.3113894394960690093 ) ) ;
#2180 = APPROVAL_PERSON_ORGANIZATION ( #4447, #4769, #2511 ) ;
#2181 = VERTEX_POINT ( 'NONE', #19997 ) ;
#2182 = DIRECTION ( 'NONE',  ( -0.8660254037844361541, 0.000000000000000000, -0.5000000000000042188 ) ) ;
#2183 = ORIENTED_EDGE ( 'NONE', *, *, #14379, .T. ) ;
#2184 = CARTESIAN_POINT ( 'NONE',  ( -0.2777741477604763753, 4.117533257858705831, 0.1469810680412119430 ) ) ;
#2185 = VECTOR ( 'NONE', #10205, 39.37007874015748143 ) ;
#2186 = CARTESIAN_POINT ( 'NONE',  ( 0.0007708829432935857895, 4.654922335358357088, -0.3119992858245870804 ) ) ;
#2187 = CARTESIAN_POINT ( 'NONE',  ( -0.2230971623002954152, -0.2230971623002953874, -0.1495138888888886963 ) ) ;
#2188 = CARTESIAN_POINT ( 'NONE',  ( 0.000000000000000000, 0.000000000000000000, 1.326383476483184332 ) ) ;
#2189 = CARTESIAN_POINT ( 'NONE',  ( 0.3028046083902323216, 5.145323248153195195, 0.02283065314510586419 ) ) ;
#2190 = ORIENTED_EDGE ( 'NONE', *, *, #21670, .T. ) ;
#2191 = LOCAL_TIME ( 21, 9, 13.00000000000000000, #22478 ) ;
#2192 = CARTESIAN_POINT ( 'NONE',  ( -0.2233192592356399442, -0.05267857152611380572, -0.3073725909049500049 ) ) ;
#2193 = CARTESIAN_POINT ( 'NONE',  ( -5.178964085587577574E-17, 0.5770833332574667462, 0.2819296736111110979 ) ) ;
#2194 = CARTESIAN_POINT ( 'NONE',  ( 0.1954553509668047195, 0.1954553509668046085, -0.09222222222222178911 ) ) ;
#2195 = CARTESIAN_POINT ( 'NONE',  ( 0.2982755344125032071, 0.5726520937526655697, -1.097998983683558638 ) ) ;
#2196 = DIRECTION ( 'NONE',  ( -1.000000000000000000, 0.000000000000000000, 0.000000000000000000 ) ) ;
#2197 = CARTESIAN_POINT ( 'NONE',  ( 0.1144950937579609085, -0.2764156081756484751, 0.1126388888888909395 ) ) ;
#2198 = VERTEX_POINT ( 'NONE', #1701 ) ;
#2199 = DIRECTION ( 'NONE',  ( -0.000000000000000000, 0.9961946980917454342, -0.08715574274765824914 ) ) ;
#2200 = CARTESIAN_POINT ( 'NONE',  ( 0.006454613307746654219, 0.5491961284534641052, 0.04193467568257214922 ) ) ;
#2201 = CARTESIAN_POINT ( 'NONE',  ( 0.3119999999999999996, 0.3548611111111107386, -0.1292346314604056468 ) ) ;
#2202 = CARTESIAN_POINT ( 'NONE',  ( 5.731347020009612645E-17, 5.231333333333332725, 0.3119999999999999996 ) ) ;
#2203 =( REPRESENTATION_RELATIONSHIP ('NONE','NONE', #4490, #16955 ) REPRESENTATION_RELATIONSHIP_WITH_TRANSFORMATION ( #21846 )SHAPE_REPRESENTATION_RELATIONSHIP( ) );
#2204 = AXIS2_PLACEMENT_3D ( 'NONE', #10215, #8851, #1299 ) ;
#2205 = CARTESIAN_POINT ( 'NONE',  ( -1.726321361862525858E-17, 4.297305555631421470, -0.2819296736111110979 ) ) ;
#2206 = CARTESIAN_POINT ( 'NONE',  ( -0.08161796258724582365, 4.347022020324052605, 0.3038890204011986951 ) ) ;
#2207 = CYLINDRICAL_SURFACE ( 'NONE', #5585, 0.3119999999999999996 ) ;
#2208 = ORIENTED_EDGE ( 'NONE', *, *, #10822, .T. ) ;
#2209 = CARTESIAN_POINT ( 'NONE',  ( 0.06335377612981493711, 0.3036162241458739697, 0.3999999999999999667 ) ) ;
#2210 = CARTESIAN_POINT ( 'NONE',  ( 0.1993543840281267465, 4.929250000075866112, 0.1993543840281266633 ) ) ;
#2211 = CARTESIAN_POINT ( 'NONE',  ( 0.3613381517857143232, 0.4187499999024575370, 0.1174058825155741975 ) ) ;
#2212 = LOCAL_TIME ( 21, 9, 13.00000000000000000, #19750 ) ;
#2213 = CARTESIAN_POINT ( 'NONE',  ( -0.2504139486751147947, 5.150879149016799552, -0.1698805244519268065 ) ) ;
#2214 =( NAMED_UNIT ( * ) PLANE_ANGLE_UNIT ( ) SI_UNIT ( $, .RADIAN. ) );
#2215 = CARTESIAN_POINT ( 'NONE',  ( 0.4795759075923629045, -0.04315724733464136598, 0.07439896364133659346 ) ) ;
#2216 = CARTESIAN_POINT ( 'NONE',  ( -1.562282291722813840E-15, 0.000000000000000000, -2.540999999999999037 ) ) ;
#2217 = AXIS2_PLACEMENT_3D ( 'NONE', #5357, #10982, #8773 ) ;
#2218 = CARTESIAN_POINT ( 'NONE',  ( 0.2819296736111111534, 4.391055555631421470, 0.1167790944451422563 ) ) ;
#2219 = CARTESIAN_POINT ( 'NONE',  ( -0.3136059260014000261, 4.058353895888922480, 0.02336461472333654921 ) ) ;
#2220 = CARTESIAN_POINT ( 'NONE',  ( 0.2764156081756484196, -5.077672346800151106E-17, 0.01194444444444569750 ) ) ;
#2221 = CARTESIAN_POINT ( 'NONE',  ( -5.178964085587577574E-17, 0.5354166665908000056, 0.2819296736111110979 ) ) ;
#2222 = ORIENTED_EDGE ( 'NONE', *, *, #97, .F. ) ;
#2223 = CARTESIAN_POINT ( 'NONE',  ( -0.1167790944451424368, 0.5319444443685777957, 0.2819296736111110424 ) ) ;
#2224 = CARTESIAN_POINT ( 'NONE',  ( 0.2206173157302028787, 4.127166666666665762, 0.2206173157302027954 ) ) ;
#2225 = CARTESIAN_POINT ( 'NONE',  ( 0.000000000000000000, 5.384999999999999787, 0.000000000000000000 ) ) ;
#2226 = CARTESIAN_POINT ( 'NONE',  ( 0.2472135954999579721, 0.2678571428571427382, -0.3402603233408159622 ) ) ;
#2227 = CARTESIAN_POINT ( 'NONE',  ( -0.1306872919485615459, -0.3155070326520293400, 0.1838194444444468667 ) ) ;
#2228 = CARTESIAN_POINT ( 'NONE',  ( -0.08339729271158345669, -0.4931164279685558149, 0.07808165802386347887 ) ) ;
#2229 = DIRECTION ( 'NONE',  ( 0.4999999999999997224, 0.8660254037844388186, -0.000000000000000000 ) ) ;
#2230 = CARTESIAN_POINT ( 'NONE',  ( 0.1167790944451423119, 0.4902777777019112215, -0.2819296736111110979 ) ) ;
#2231 = CARTESIAN_POINT ( 'NONE',  ( -0.1993543840281267465, 0.2923611110352445364, 0.1993543840281266633 ) ) ;
#2232 = CARTESIAN_POINT ( 'NONE',  ( 0.2819296736111110424, 4.231333333409199149, -0.1167790944451423396 ) ) ;
#2233 = CARTESIAN_POINT ( 'NONE',  ( 0.3999999999999999667, 0.3232142855192008946, -0.1299678784931625475 ) ) ;
#2234 = CARTESIAN_POINT ( 'NONE',  ( 0.1993543840281266633, 4.901472222298088433, -0.1993543840281266910 ) ) ;
#2235 = EDGE_CURVE ( 'NONE', #19908, #12402, #24004, .T. ) ;
#2236 = CARTESIAN_POINT ( 'NONE',  ( -0.1167790944451423119, 4.509111111186976828, -0.2819296736111110979 ) ) ;
#2237 = CARTESIAN_POINT ( 'NONE',  ( 0.2209708691207961095, -0.2209708691207961651, 0.3105555555555593039 ) ) ;
#2238 = CIRCLE ( 'NONE', #5338, 0.2041999999999999926 ) ;
#2239 = CARTESIAN_POINT ( 'NONE',  ( -0.04810232026111291304, 0.5134939898139645464, 0.05816208736419732628 ) ) ;
#2240 = CARTESIAN_POINT ( 'NONE',  ( 0.1292346314604056190, 4.040361111262843252, -0.3119999999999999996 ) ) ;
#2241 = CARTESIAN_POINT ( 'NONE',  ( 3.820898013339742174E-17, 5.384999999999999787, 0.3119999999999999996 ) ) ;
#2242 = CARTESIAN_POINT ( 'NONE',  ( 0.000000000000000000, 5.384999999999999787, -0.3119999999999999996 ) ) ;
#2243 = ORIENTED_EDGE ( 'NONE', *, *, #7426, .T. ) ;
#2244 = APPROVAL_ROLE ( '' ) ;
#2245 = CARTESIAN_POINT ( 'NONE',  ( 0.2759399609360094763, 0.05657080772233213928, 0.3928742422042607596 ) ) ;
#2246 = CARTESIAN_POINT ( 'NONE',  ( -0.02441201398334205686, 3.066692553488282957, 3.451468604327566858 ) ) ;
#2247 = CARTESIAN_POINT ( 'NONE',  ( 1.910449006669871087E-17, 0.5319444444444439979, -0.3119999999999999996 ) ) ;
#2248 = ORIENTED_EDGE ( 'NONE', *, *, #11014, .F. ) ;
#2249 = CARTESIAN_POINT ( 'NONE',  ( 0.1292346314604057023, 0.5006944442927115935, 0.3119999999999998885 ) ) ;
#2250 = VECTOR ( 'NONE', #8689, 39.37007874015748143 ) ;
#2251 = CARTESIAN_POINT ( 'NONE',  ( 0.1852222081618724869, 4.260541747846676941, -0.2521104950801930089 ) ) ;
#2252 = CARTESIAN_POINT ( 'NONE',  ( 0.4224645524279259101, 0.2973558542979368169, 0.3902541392329166858 ) ) ;
#2253 = DIRECTION ( 'NONE',  ( 0.000000000000000000, 1.000000000000000000, 0.000000000000000000 ) ) ;
#2254 = CARTESIAN_POINT ( 'NONE',  ( 0.2923287055106771337, 0.07232142847388615958, -0.2123892367102620249 ) ) ;
#2255 = CARTESIAN_POINT ( 'NONE',  ( 0.2895852664652339703, 5.177710075864474071, 0.05112040707668003697 ) ) ;
#2256 = CC_DESIGN_PERSON_AND_ORGANIZATION_ASSIGNMENT ( #19331, #436, ( #582 ) ) ;
#2257 = VERTEX_POINT ( 'NONE', #9139 ) ;
#2258 = CARTESIAN_POINT ( 'NONE',  ( 0.2233192592356400275, 0.3794642856167432798, -0.3073725909049499494 ) ) ;
#2259 = FACE_OUTER_BOUND ( 'NONE', #13993, .T. ) ;
#2260 = CARTESIAN_POINT ( 'NONE',  ( 0.1954553509668047195, 0.1954553509668046085, 0.4563888888888936735 ) ) ;
#2261 = CARTESIAN_POINT ( 'NONE',  ( 0.2819296736111110424, 3.939666666742531742, -0.1167790944451423396 ) ) ;
#2262 = CARTESIAN_POINT ( 'NONE',  ( -0.1568404389086238138, -0.4507140077415615065, 0.4133480672484174390 ) ) ;
#2263 = CARTESIAN_POINT ( 'NONE',  ( 0.02013700421290525247, 5.118816490325227342, 0.3086180630080335718 ) ) ;
#2264 = FACE_OUTER_BOUND ( 'NONE', #10072, .T. ) ;
#2265 = CARTESIAN_POINT ( 'NONE',  ( -0.3119999999999998885, 4.838972222373953969, 0.1292346314604058410 ) ) ;
#2266 = CARTESIAN_POINT ( 'NONE',  ( 0.1993543840281266633, 4.957027777853642903, -0.1993543840281266910 ) ) ;
#2267 = ORIENTED_EDGE ( 'NONE', *, *, #3707, .T. ) ;
#2268 = CARTESIAN_POINT ( 'NONE',  ( 0.2819296736111110979, 4.325083333409198261, -3.452642723725051716E-17 ) ) ;
#2269 = CIRCLE ( 'NONE', #3021, 0.3253415854805813412 ) ;
#2270 = CARTESIAN_POINT ( 'NONE',  ( 0.3613381517857143232, 0.06874999990245758696, -0.1174058825155740587 ) ) ;
#2271 = ORIENTED_EDGE ( 'NONE', *, *, #6162, .F. ) ;
#2272 = EDGE_CURVE ( 'NONE', #12608, #15982, #20119, .T. ) ;
#2273 = VERTEX_POINT ( 'NONE', #14766 ) ;
#2274 = COORDINATED_UNIVERSAL_TIME_OFFSET ( 0, 0, .AHEAD. ) ;
#2275 = CARTESIAN_POINT ( 'NONE',  ( -0.2230971623002953874, 0.2230971623002954152, 0.4477083333333382598 ) ) ;
#2276 = FACE_OUTER_BOUND ( 'NONE', #15465, .T. ) ;
#2277 = CARTESIAN_POINT ( 'NONE',  ( -0.1993543840281266355, 3.929250000075865668, 0.1993543840281267465 ) ) ;
#2278 = CARTESIAN_POINT ( 'NONE',  ( 0.07073318196858055518, 4.430697953807255729, -0.3040470679591011915 ) ) ;
#2280 = EDGE_CURVE ( 'NONE', #20305, #19663, #10409, .T. ) ;
#2279 = DIRECTION ( 'NONE',  ( 0.4999999999999915068, 0.000000000000000000, -0.8660254037844434816 ) ) ;
#2281 = B_SPLINE_CURVE_WITH_KNOTS ( 'NONE', 1,
 ( #17512, #807 ),
 .UNSPECIFIED., .F., .F.,
 ( 2, 2 ),
 ( 0.000000000000000000, 1.000000000000000000 ),
 .UNSPECIFIED. ) ;
#2282 = CARTESIAN_POINT ( 'NONE',  ( 0.4206390790005973823, -0.2984097918724726850, 0.05816431335568269384 ) ) ;
#2283 = ORIENTED_EDGE ( 'NONE', *, *, #4095, .T. ) ;
#2284 = CARTESIAN_POINT ( 'NONE',  ( 0.1954553509668047195, 0.1954553509668046085, 0.2341666666666697150 ) ) ;
#2285 = CARTESIAN_POINT ( 'NONE',  ( 0.1993543840281266355, 0.5423611110352445364, 0.1993543840281267465 ) ) ;
#2286 = CARTESIAN_POINT ( 'NONE',  ( -0.1954553509668046640, 0.1954553509668046918, 0.4772222222222271548 ) ) ;
#2287 = CARTESIAN_POINT ( 'NONE',  ( -0.1167790944451423257, 4.689666666742532186, -0.2819296736111110424 ) ) ;
#2288 = CARTESIAN_POINT ( 'NONE',  ( -0.3119999999999999996, 3.939666666666666206, 0.000000000000000000 ) ) ;
#2289 = CARTESIAN_POINT ( 'NONE',  ( 0.1167790944451424368, 4.759111111186977716, 0.2819296736111110424 ) ) ;
#2290 = CARTESIAN_POINT ( 'NONE',  ( -0.2759399609360070338, 0.05657080772233105681, -0.07037424220425755883 ) ) ;
#2291 = CARTESIAN_POINT ( 'NONE',  ( -0.1868639192671616156, 4.559812086079793048, -3.228500364337124395 ) ) ;
#2292 = CARTESIAN_POINT ( 'NONE',  ( -0.1534580259519314760, -1.109535145422194601E-16, 0.3483058538587986974 ) ) ;
#2293 = CARTESIAN_POINT ( 'NONE',  ( -0.05329418186028045401, 1.034028482145805672, -2.997150792794772922 ) ) ;
#2294 = CARTESIAN_POINT ( 'NONE',  ( 0.2206173157302028787, 4.516055555555555046, 0.2206173157302027954 ) ) ;
#2295 = CARTESIAN_POINT ( 'NONE',  ( 0.2819296736111111534, 3.821611111186975940, 0.1167790944451422563 ) ) ;
#2296 = CARTESIAN_POINT ( 'NONE',  ( 0.01055874796617838236, 4.987974962125321987, -0.3118467276096589247 ) ) ;
#2297 = ORIENTED_EDGE ( 'NONE', *, *, #6038, .F. ) ;
#2298 = CARTESIAN_POINT ( 'NONE',  ( 0.3806690758928571450, 0.4513392855679720372, 0.000000000000000000 ) ) ;
#2299 = ORIENTED_EDGE ( 'NONE', *, *, #3851, .F. ) ;
#2300 =( BOUNDED_CURVE ( )  B_SPLINE_CURVE ( 2, ( #20741, #15500, #9528, #19150, #16961, #17326, #7927, #256, #5860 ),
 .UNSPECIFIED., .F., .F. ) 
 B_SPLINE_CURVE_WITH_KNOTS ( ( 3, 2, 2, 2, 3 ),
 ( 0.6160714285714284921, 0.6205357142857141906, 0.6250000000000000000, 0.6294642857142856984, 0.6339285714285713969 ),
 .UNSPECIFIED. ) 
 CURVE ( )  GEOMETRIC_REPRESENTATION_ITEM ( )  RATIONAL_B_SPLINE_CURVE ( ( 1.000000000000001998, 0.9238795325112848511, 1.000000000000000000, 0.9238795325112867385, 1.000000000000000000, 0.9238795325112867385, 1.000000000000000000, 0.9238795325112867385, 1.000000000000000000 ) ) 
 REPRESENTATION_ITEM ( '' )  );
#2301 =( BOUNDED_CURVE ( )  B_SPLINE_CURVE ( 2, ( #12414, #18366, #14475, #14597, #24085, #7035, #8978, #9093, #14349 ),
 .UNSPECIFIED., .F., .F. ) 
 B_SPLINE_CURVE_WITH_KNOTS ( ( 3, 2, 2, 2, 3 ),
 ( 0.2589285714285712303, 0.2633928571428569287, 0.2678571428571426827, 0.2723214285714283811, 0.2767857142857141350 ),
 .UNSPECIFIED. ) 
 CURVE ( )  GEOMETRIC_REPRESENTATION_ITEM ( )  RATIONAL_B_SPLINE_CURVE ( ( 1.000000000000003775, 0.9238795325112829637, 1.000000000000000000, 0.9238795325112867385, 1.000000000000000000, 0.9238795325112867385, 1.000000000000000000, 0.9238795325112896251, 0.9999999999999971134 ) ) 
 REPRESENTATION_ITEM ( '' )  );
#2302 = CARTESIAN_POINT ( 'NONE',  ( 0.2874800067704069706, 4.700142690845275695, -0.1212674689108930587 ) ) ;
#2303 = DIRECTION ( 'NONE',  ( 0.000000000000000000, 0.000000000000000000, 1.000000000000000000 ) ) ;
#2304 = CARTESIAN_POINT ( 'NONE',  ( 0.2230971623002953874, -0.2230971623002954429, -0.1356249999999996902 ) ) ;
#2305 = CARTESIAN_POINT ( 'NONE',  ( -0.04074214740764643683, 3.933880325120055144, -0.3094968904035911850 ) ) ;
#2306 = EDGE_CURVE ( 'NONE', #2198, #11353, #16778, .T. ) ;
#2307 = ORIENTED_EDGE ( 'NONE', *, *, #5269, .T. ) ;
#2308 = CARTESIAN_POINT ( 'NONE',  ( -0.3613381517857143232, 0.1008928570453147405, -4.425116109941954795E-17 ) ) ;
#2309 = CARTESIAN_POINT ( 'NONE',  ( -0.2819296736111110424, 0.5597222221463555858, -0.1167790944451423396 ) ) ;
#2310 = CARTESIAN_POINT ( 'NONE',  ( -0.2764156081756484196, -0.1144950937579609362, -0.1234722222222220528 ) ) ;
#2311 = CARTESIAN_POINT ( 'NONE',  ( 0.08213261185791022323, 0.1892061861790486077, -1.237979020847294276 ) ) ;
#2312 = DIRECTION ( 'NONE',  ( -0.000000000000000000, -1.000000000000000000, -0.000000000000000000 ) ) ;
#2313 = CARTESIAN_POINT ( 'NONE',  ( 0.2764156081756483641, -0.1144950937579611167, 0.1751388888888914530 ) ) ;
#2314 = CARTESIAN_POINT ( 'NONE',  ( -0.3002551575529973094, 4.610724490433781853, -0.08857506410196538948 ) ) ;
#2315 = CARTESIAN_POINT ( 'NONE',  ( -0.01848103877824625041, 0.5441716683897389606, 0.04413116910601661003 ) ) ;
#2316 = CARTESIAN_POINT ( 'NONE',  ( 0.000000000000000000, 5.072999999999999510, 0.000000000000000000 ) ) ;
#2317 = CARTESIAN_POINT ( 'NONE',  ( 1.910449006669871087E-17, 0.2541666666666663188, -0.3119999999999999996 ) ) ;
#2318 = CARTESIAN_POINT ( 'NONE',  ( -0.1292346314604057023, 5.116749999999999687, 0.3119999999999998885 ) ) ;
#2319 = CIRCLE ( 'NONE', #741, 0.3425000000000000266 ) ;
#2320 = CARTESIAN_POINT ( 'NONE',  ( -0.1167790944451423535, 4.154944444520309865, 0.2819296736111110424 ) ) ;
#2321 = CARTESIAN_POINT ( 'NONE',  ( -0.2725090806957128353, 4.340125742647720664, 0.1573274259844539558 ) ) ;
#2322 = CARTESIAN_POINT ( 'NONE',  ( 0.3950000000000000178, 2.740039370078740433, -2.591000000000000192 ) ) ;
#2323 = EDGE_CURVE ( 'NONE', #11539, #7602, #3410, .T. ) ;
#2324 = DIRECTION ( 'NONE',  ( 8.659560562354953812E-17, -0.7071067811865459074, 0.7071067811865492381 ) ) ;
#2325 = EDGE_LOOP ( 'NONE', ( #2485, #13346, #16518 ) ) ;
#2326 = CARTESIAN_POINT ( 'NONE',  ( 0.3236067977499790249, 0.3267857140906293978, -0.2351141009169892826 ) ) ;
#2327 = CARTESIAN_POINT ( 'NONE',  ( 0.1167790944451424368, 4.648000000075865223, 0.2819296736111110424 ) ) ;
#2328 = CARTESIAN_POINT ( 'NONE',  ( 0.1583529533612939577, 0.4498407571151590290, 0.08855978515308939036 ) ) ;
#2329 = ADVANCED_FACE ( 'NONE', ( #8900 ), #15083, .T. ) ;
#2330 = CARTESIAN_POINT ( 'NONE',  ( 0.7108475124358174524, 3.066692553488282957, 2.927961747820534644 ) ) ;
#2331 = EDGE_CURVE ( 'NONE', #9441, #10582, #7669, .T. ) ;
#2332 = ADVANCED_FACE ( 'NONE', ( #16702 ), #14396, .T. ) ;
#2333 = CARTESIAN_POINT ( 'NONE',  ( 0.000000000000000000, 0.000000000000000000, 0.000000000000000000 ) ) ;
#2334 = FACE_OUTER_BOUND ( 'NONE', #3057, .T. ) ;
#2335 = CARTESIAN_POINT ( 'NONE',  ( 0.1954553509668047195, 0.1954553509668046085, -0.09916666666666627827 ) ) ;
#2336 = CIRCLE ( 'NONE', #21403, 1.223000000000000309 ) ;
#2337 = CARTESIAN_POINT ( 'NONE',  ( -0.2819296736111110424, 4.203555555631421470, 0.1167790944451424923 ) ) ;
#2338 = DATE_AND_TIME ( #9649, #22054 ) ;
#2339 = EDGE_CURVE ( 'NONE', #5324, #9833, #14882, .T. ) ;
#2340 = CARTESIAN_POINT ( 'NONE',  ( -0.01317391978361341122, 4.044190193732460692, -0.3117386529996676869 ) ) ;
#2341 = CARTESIAN_POINT ( 'NONE',  ( 0.2764156081756483641, -0.1144950937579611028, 0.06402777777777945989 ) ) ;
#2342 = FACE_OUTER_BOUND ( 'NONE', #9167, .T. ) ;
#2343 = CARTESIAN_POINT ( 'NONE',  ( -0.1167790944451422702, 0.3444444443685777402, -0.2819296736111110424 ) ) ;
#2344 = CARTESIAN_POINT ( 'NONE',  ( 0.000000000000000000, 0.000000000000000000, 1.326383476483184332 ) ) ;
#2345 = CARTESIAN_POINT ( 'NONE',  ( -0.2272226533539420668, 5.205980271775564105, 0.1697100602738888242 ) ) ;
#2346 = CARTESIAN_POINT ( 'NONE',  ( -0.4000000000000000222, 0.2928571428571427604, -4.898587196589413075E-17 ) ) ;
#2347 = CARTESIAN_POINT ( 'NONE',  ( -0.1306872919485615459, -0.3155070326520293400, 0.1282638888888908979 ) ) ;
#2348 = CARTESIAN_POINT ( 'NONE',  ( -1.906863420619159052E-17, 5.092106365077719410, -0.3114144293598434809 ) ) ;
#2349 = LINE ( 'NONE', #7706, #20263 ) ;
#2350 = CARTESIAN_POINT ( 'NONE',  ( 0.2819296736111110424, 0.5874999999241333759, 0.1167790944451424923 ) ) ;
#2351 = CARTESIAN_POINT ( 'NONE',  ( 0.2819296736111110979, 0.2576388888130222155, 0.000000000000000000 ) ) ;
#2352 = CARTESIAN_POINT ( 'NONE',  ( -0.1993543840281266355, 4.373694444520309865, 0.1993543840281267465 ) ) ;
#2353 = CARTESIAN_POINT ( 'NONE',  ( 0.3999999999999999667, 0.2446428569477723525, 0.1299678784931626307 ) ) ;
#2354 = CARTESIAN_POINT ( 'NONE',  ( -0.2819296736111110979, 4.811194444520309865, 0.000000000000000000 ) ) ;
#2355 = CARTESIAN_POINT ( 'NONE',  ( 0.1167790944451424506, 4.259111111186976828, 0.2819296736111110424 ) ) ;
#2356 = CIRCLE ( 'NONE', #1575, 0.3525000000000007017 ) ;
#2357 = CARTESIAN_POINT ( 'NONE',  ( 0.1294417382415921358, -0.3125000000000002220, 0.3070833333333370940 ) ) ;
#2358 = AXIS2_PLACEMENT_3D ( 'NONE', #17220, #1982, #22460 ) ;
#2359 = CARTESIAN_POINT ( 'NONE',  ( -0.09134320533038761680, 0.5015400784327411765, 0.06108448616841834905 ) ) ;
#2360 = CARTESIAN_POINT ( 'NONE',  ( -0.1292346314604056745, 3.880638889040620931, -0.3119999999999999996 ) ) ;
#2361 = CARTESIAN_POINT ( 'NONE',  ( 0.2206173157302027676, 0.1222222222222218990, 0.2206173157302028787 ) ) ;
#2362 = CARTESIAN_POINT ( 'NONE',  ( 0.000000000000000000, 2.740000000000000213, -0.05000000000000028727 ) ) ;
#2363 = ORIENTED_EDGE ( 'NONE', *, *, #14733, .T. ) ;
#2364 = EDGE_CURVE ( 'NONE', #18643, #2744, #14516, .T. ) ;
#2365 = DATE_TIME_ROLE ( 'classification_date' ) ;
#2366 = VERTEX_POINT ( 'NONE', #16226 ) ;
#2367 = DIRECTION ( 'NONE',  ( 0.000000000000000000, 0.000000000000000000, -1.000000000000000000 ) ) ;
#2368 = CIRCLE ( 'NONE', #11329, 0.09499999999999995948 ) ;
#2369 = CARTESIAN_POINT ( 'NONE',  ( -0.01584329491212002269, 0.03242967361111059876, 0.2819296736111481794 ) ) ;
#2370 = LINE ( 'NONE', #11516, #12422 ) ;
#2371 = ORIENTED_EDGE ( 'NONE', *, *, #6180, .T. ) ;
#2372 = CARTESIAN_POINT ( 'NONE',  ( -0.2819296736111110424, 0.1291666665908000611, -0.1167790944451423396 ) ) ;
#2373 = CONICAL_SURFACE ( 'NONE', #20279, 0.4453125000000000000, 1.047197551196600074 ) ;
#2374 = ORIENTED_EDGE ( 'NONE', *, *, #7635, .F. ) ;
#2375 = CARTESIAN_POINT ( 'NONE',  ( 0.06082884619916966579, 4.264387106092869750, -0.3064377004203949206 ) ) ;
#2376 = CARTESIAN_POINT ( 'NONE',  ( 0.2091198842963235827, 0.4097039017751566425, 0.4343513344076809224 ) ) ;
#2377 = DIRECTION ( 'NONE',  ( 0.000000000000000000, -0.000000000000000000, 1.000000000000000000 ) ) ;
#2378 = CARTESIAN_POINT ( 'NONE',  ( 0.3613381517857143232, 0.1366071427596004251, 0.000000000000000000 ) ) ;
#2379 = CARTESIAN_POINT ( 'NONE',  ( 1.222470958122163998, 2.291712385858715173, -0.8172771125692949168 ) ) ;
#2380 = ORIENTED_EDGE ( 'NONE', *, *, #12493, .F. ) ;
#2381 = CARTESIAN_POINT ( 'NONE',  ( 0.1116596296178199027, 0.3544642856167432576, 0.3436530038418508792 ) ) ;
#2382 = CARTESIAN_POINT ( 'NONE',  ( 0.3125000000000000000, -5.740531871003217465E-17, -0.02277777777777697382 ) ) ;
#2383 = CARTESIAN_POINT ( 'NONE',  ( -3.385114897866767815E-17, -0.2764156081756484196, 0.4355555555555601921 ) ) ;
#2384 = CARTESIAN_POINT ( 'NONE',  ( 0.1993543840281267465, 3.984805555631421470, 0.1993543840281266633 ) ) ;
#2385 = CARTESIAN_POINT ( 'NONE',  ( -0.2139474665362521011, -0.4177432499681407729, 0.4289390872834994428 ) ) ;
#2386 = CARTESIAN_POINT ( 'NONE',  ( -0.1295556563484780987, 5.167372147454906361, -0.2683632288998299420 ) ) ;
#2387 = CARTESIAN_POINT ( 'NONE',  ( -0.1292346314604057023, 4.845916666818398610, 0.3119999999999998885 ) ) ;
#2388 = CARTESIAN_POINT ( 'NONE',  ( -0.1167790944451423535, 4.988277777853643791, 0.2819296736111110979 ) ) ;
#2389 = ORIENTED_EDGE ( 'NONE', *, *, #11086, .F. ) ;
#2390 = VECTOR ( 'NONE', #14299, 39.37007874015748143 ) ;
#2391 = CARTESIAN_POINT ( 'NONE',  ( -0.2819296736111110979, 4.186194444520309865, 0.000000000000000000 ) ) ;
#2392 = ORIENTED_EDGE ( 'NONE', *, *, #22273, .F. ) ;
#2393 = CARTESIAN_POINT ( 'NONE',  ( -0.2923287055106771337, 0.1651785713310290060, -0.2123892367102620804 ) ) ;
#2394 = ORIENTED_EDGE ( 'NONE', *, *, #7688, .T. ) ;
#2395 = ORIENTED_EDGE ( 'NONE', *, *, #5929, .T. ) ;
#2396 = APPROVAL_STATUS ( 'not_yet_approved' ) ;
#2397 = DIRECTION ( 'NONE',  ( 0.000000000000000000, 0.000000000000000000, 1.000000000000000000 ) ) ;
#2398 = CARTESIAN_POINT ( 'NONE',  ( 0.2206173157302027676, 0.2888888888888885287, 0.2206173157302028787 ) ) ;
#2399 = CARTESIAN_POINT ( 'NONE',  ( -0.2819296736111110424, 3.870222222298087988, 0.1167790944451424923 ) ) ;
#2400 = CARTESIAN_POINT ( 'NONE',  ( 0.1066988909913641620, 4.429648004107447967, -0.2931885909852042782 ) ) ;
#2401 = CARTESIAN_POINT ( 'NONE',  ( -3.827021247335479543E-17, -0.3125000000000000000, -0.08527777777777710566 ) ) ;
#2402 = CARTESIAN_POINT ( 'NONE',  ( 0.3096487991955518826, -0.3624900597954727743, 0.07655254331175391502 ) ) ;
#2403 = CARTESIAN_POINT ( 'NONE',  ( 0.000000000000000000, 0.2764156081756484196, 0.2966666666666702423 ) ) ;
#2404 = CARTESIAN_POINT ( 'NONE',  ( 0.1993543840281266910, 0.4451388888130222710, -0.1993543840281266910 ) ) ;
#2405 = CARTESIAN_POINT ( 'NONE',  ( -0.1144950937579609779, 0.2764156081756484196, -0.1443055555555555203 ) ) ;
#2406 = ORIENTED_EDGE ( 'NONE', *, *, #20795, .T. ) ;
#2407 = CARTESIAN_POINT ( 'NONE',  ( -0.2819296736111110979, 4.644527777853643791, 0.000000000000000000 ) ) ;
#2408 = CARTESIAN_POINT ( 'NONE',  ( -0.3119999999999998885, 3.943138888888888083, 0.1292346314604058410 ) ) ;
#2409 = CARTESIAN_POINT ( 'NONE',  ( -0.1167790944451423535, 4.696611111186976828, 0.2819296736111110424 ) ) ;
#2410 = CARTESIAN_POINT ( 'NONE',  ( 1.222470958122163998, 2.978485840173427324, -0.8773620042323713175 ) ) ;
#2411 = CARTESIAN_POINT ( 'NONE',  ( -0.3124999999999989453, -0.1294417382415932460, 0.3418055555555593039 ) ) ;
#2412 = CARTESIAN_POINT ( 'NONE',  ( 0.1355891867880099633, -6.434570819605719236E-16, 0.3400430461746979938 ) ) ;
#2413 = CARTESIAN_POINT ( 'NONE',  ( 0.3119999999999999996, 4.304249999999999687, -0.1292346314604056745 ) ) ;
#2414 = CARTESIAN_POINT ( 'NONE',  ( -0.06335377612981410445, 0.3088837756590411265, 0.4000000000000001887 ) ) ;
#2415 = DIRECTION ( 'NONE',  ( 1.000000000000000000, 0.000000000000000000, 0.000000000000000000 ) ) ;
#2416 = EDGE_LOOP ( 'NONE', ( #16813, #7601, #6395 ) ) ;
#2417 = DIRECTION ( 'NONE',  ( -0.000000000000000000, -1.000000000000000000, -0.000000000000000000 ) ) ;
#2418 = ORIENTED_EDGE ( 'NONE', *, *, #18544, .F. ) ;
#2419 = PRODUCT_RELATED_PRODUCT_CATEGORY ( 'detail', '', ( #3495 ) ) ;
#2420 = ADVANCED_FACE ( 'NONE', ( #22300 ), #5597, .T. ) ;
#2421 = CARTESIAN_POINT ( 'NONE',  ( 0.2719451416848666647, 4.691957884589568195, 0.1583271517010935991 ) ) ;
#2422 = DESIGN_CONTEXT ( 'detailed design', #8883, 'design' ) ;
#2423 = CARTESIAN_POINT ( 'NONE',  ( 0.4683396222371035145, -0.2655382811872516458, 0.04698599556840714342 ) ) ;
#2424 = CARTESIAN_POINT ( 'NONE',  ( -0.2764156081756484196, 1.692557448933383907E-17, 0.3661111111111152172 ) ) ;
#2425 = DIRECTION ( 'NONE',  ( 0.000000000000000000, 0.000000000000000000, -1.000000000000000000 ) ) ;
#2426 = VERTEX_POINT ( 'NONE', #3776 ) ;
#2427 = CARTESIAN_POINT ( 'NONE',  ( 0.3613381517857143232, -0.009821428668970965531, 0.1174058825155742114 ) ) ;
#2428 = CARTESIAN_POINT ( 'NONE',  ( -0.1993543840281266633, 0.3895833332574667462, -0.1993543840281266910 ) ) ;
#2429 = CARTESIAN_POINT ( 'NONE',  ( 0.000000000000000000, 4.559812086079793048, 0.000000000000000000 ) ) ;
#2430 = CARTESIAN_POINT ( 'NONE',  ( 0.07172766006922927373, 0.7801234116097515159, -1.079864709389726452 ) ) ;
#2431 = CARTESIAN_POINT ( 'NONE',  ( 0.2206173157302028232, 0.5249999999999996891, -0.2206173157302028232 ) ) ;
#2432 = CARTESIAN_POINT ( 'NONE',  ( 0.1144950937579611444, 0.2764156081756483641, 0.1334722222222244348 ) ) ;
#2433 = CARTESIAN_POINT ( 'NONE',  ( -0.02046452715226480465, 5.117794691263952700, 0.3082562737412080089 ) ) ;
#2434 = CARTESIAN_POINT ( 'NONE',  ( 0.000000000000000000, 0.000000000000000000, 0.000000000000000000 ) ) ;
#2435 = CARTESIAN_POINT ( 'NONE',  ( 0.03742218716966667219, 4.101846522467903000E-18, -0.3789181498996747055 ) ) ;
#2436 = CARTESIAN_POINT ( 'NONE',  ( 0.1292346314604056745, 0.1951388888888886397, -0.3119999999999999996 ) ) ;
#2437 = CARTESIAN_POINT ( 'NONE',  ( 0.1292346314604056190, 5.088972222222220232, -0.3119999999999999996 ) ) ;
#2438 = EDGE_CURVE ( 'NONE', #8827, #15879, #14286, .T. ) ;
#2439 = CARTESIAN_POINT ( 'NONE',  ( 0.1993543840281267465, 4.220916666742532186, 0.1993543840281266633 ) ) ;
#2440 = CARTESIAN_POINT ( 'NONE',  ( 0.5097595264191659981, 2.291712385858714729, -0.6667552972947653478 ) ) ;
#2441 = CARTESIAN_POINT ( 'NONE',  ( -0.2481776206062810408, 0.3871563449089069908, 0.4344098397133764333 ) ) ;
#2442 = FACE_OUTER_BOUND ( 'NONE', #19762, .T. ) ;
#2443 =( BOUNDED_CURVE ( )  B_SPLINE_CURVE ( 2, ( #17108, #19173, #19055, #7715, #6120, #13588, #21000, #9914, #22595 ),
 .UNSPECIFIED., .F., .F. ) 
 B_SPLINE_CURVE_WITH_KNOTS ( ( 3, 2, 2, 2, 3 ),
 ( 0.4732142857142858094, 0.4776785714285715079, 0.4821428571428570953, 0.4866071428571427382, 0.4910714285714283811 ),
 .UNSPECIFIED. ) 
 CURVE ( )  GEOMETRIC_REPRESENTATION_ITEM ( )  RATIONAL_B_SPLINE_CURVE ( ( 0.9999999999999981126, 0.9238795325112886259, 1.000000000000000000, 0.9238795325112867385, 1.000000000000000000, 0.9238795325112867385, 1.000000000000000000, 0.9238795325112896251, 0.9999999999999971134 ) ) 
 REPRESENTATION_ITEM ( '' )  );
#2444 = ORIENTED_EDGE ( 'NONE', *, *, #3668, .T. ) ;
#2445 = ORIENTED_EDGE ( 'NONE', *, *, #19287, .T. ) ;
#2446 = CARTESIAN_POINT ( 'NONE',  ( 0.000000000000000000, 5.072999999999999510, 0.000000000000000000 ) ) ;
#2447 = CARTESIAN_POINT ( 'NONE',  ( -0.1167790944451423257, 4.675777777853642903, -0.2819296736111110424 ) ) ;
#2448 = AXIS2_PLACEMENT_3D ( 'NONE', #23614, #18147, #14366 ) ;
#2449 = EDGE_CURVE ( 'NONE', #4057, #9930, #4129, .T. ) ;
#2450 = CARTESIAN_POINT ( 'NONE',  ( 0.3613381517857143232, 0.3508928570453146989, 0.000000000000000000 ) ) ;
#2451 = CARTESIAN_POINT ( 'NONE',  ( 0.3103034095256952396, -0.3621121203451557746, 0.4135550951626320026 ) ) ;
#2452 = APPLICATION_PROTOCOL_DEFINITION ( 'international standard', 'config_control_design', 1994, #9823 ) ;
#2453 = CARTESIAN_POINT ( 'NONE',  ( 1.573500000000000343, 0.000000000000000000, -0.1650000000000001465 ) ) ;
#2454 = CARTESIAN_POINT ( 'NONE',  ( -0.3065849364905382513, 4.708020935245015622E-15, -0.09575160315720471216 ) ) ;
#2455 = CARTESIAN_POINT ( 'NONE',  ( 5.178964085587577574E-17, 4.380638888964754507, 0.2819296736111110979 ) ) ;
#2456 = PERSON_AND_ORGANIZATION_ROLE ( 'classification_officer' ) ;
#2457 = CARTESIAN_POINT ( 'NONE',  ( -0.2917836889767269626, 4.054536616146934946, -0.1122327437212481960 ) ) ;
#2458 = CARTESIAN_POINT ( 'NONE',  ( -0.2084225359521647558, -0.1824881659814446000, -0.06500058086764819165 ) ) ;
#2459 = LINE ( 'NONE', #19271, #16491 ) ;
#2460 = CARTESIAN_POINT ( 'NONE',  ( -0.1167790944451424368, 0.3652777777019111105, 0.2819296736111110424 ) ) ;
#2461 = CARTESIAN_POINT ( 'NONE',  ( 0.1292346314604080892, 4.144527777777776478, -0.3119999999999975016 ) ) ;
#2462 = DIRECTION ( 'NONE',  ( 0.000000000000000000, 1.000000000000000000, 0.000000000000000000 ) ) ;
#2463 = LINE ( 'NONE', #6228, #4103 ) ;
#2464 = CARTESIAN_POINT ( 'NONE',  ( -3.863846776457871776E-17, -0.3155070326520292845, 0.07618055555555713898 ) ) ;
#2465 = AXIS2_PLACEMENT_3D ( 'NONE', #4945, #12289, #19463 ) ;
#2466 = CARTESIAN_POINT ( 'NONE',  ( 0.000000000000000000, 0.05000000000000028727, -2.986000000000000210 ) ) ;
#2467 = EDGE_CURVE ( 'NONE', #7539, #16753, #22901, .T. ) ;
#2468 = DIRECTION ( 'NONE',  ( -1.000000000000000000, 0.000000000000000000, -0.000000000000000000 ) ) ;
#2469 = CARTESIAN_POINT ( 'NONE',  ( 0.2819296736111110979, 0.4833333332574666907, -0.1167790944451422980 ) ) ;
#2470 = CARTESIAN_POINT ( 'NONE',  ( 0.1993543840281266910, 0.2645833332574666907, -0.1993543840281266910 ) ) ;
#2471 = EDGE_CURVE ( 'NONE', #11248, #18852, #19867, .T. ) ;
#2472 = EDGE_CURVE ( 'NONE', #22384, #13614, #15475, .T. ) ;
#2473 = CARTESIAN_POINT ( 'NONE',  ( 0.1167790944451424368, 4.217444444520310753, 0.2819296736111110424 ) ) ;
#2474 = CARTESIAN_POINT ( 'NONE',  ( 0.1236067977499789861, 0.3339285712334866263, -0.3804226065180614236 ) ) ;
#2475 = ORIENTED_EDGE ( 'NONE', *, *, #2888, .F. ) ;
#2476 = CARTESIAN_POINT ( 'NONE',  ( -0.1993543840281266355, 4.818138888964754507, 0.1993543840281267465 ) ) ;
#2477 = CARTESIAN_POINT ( 'NONE',  ( -0.1294417382415922746, -0.3125000000000000000, 0.3001388888888926743 ) ) ;
#2478 = VERTEX_POINT ( 'NONE', #20598 ) ;
#2479 = DIRECTION ( 'NONE',  ( 0.000000000000000000, 0.000000000000000000, -1.000000000000000000 ) ) ;
#2480 = CARTESIAN_POINT ( 'NONE',  ( -0.1292346314604056745, 3.936194444596176290, -0.3119999999999999996 ) ) ;
#2481 = EDGE_CURVE ( 'NONE', #1752, #8247, #12905, .T. ) ;
#2482 = FACE_OUTER_BOUND ( 'NONE', #21133, .T. ) ;
#2483 = B_SPLINE_CURVE_WITH_KNOTS ( 'NONE', 3,
 ( #22803, #371, #22684, #15254, #6095, #129, #13084, #20499, #13566, #20975, #11239, #5974, #1965, #16956, #13437, #9403, #15020 ),
 .UNSPECIFIED., .F., .F.,
 ( 4, 2, 1, 1, 1, 1, 1, 2, 2, 2, 4 ),
 ( 0.9959891374116947027, 0.9959969711276874804, 0.9960048048436802581, 0.9960204722756658136, 0.9960518071396369244, 0.9961144768675792571, 0.9962398163234638115, 0.9964904952352329204, 0.9969918530587710270, 0.9979945687058473514, 1.000000000000000000 ),
 .UNSPECIFIED. ) ;
#2484 = CIRCLE ( 'NONE', #18051, 0.001000000000000003057 ) ;
#2485 = ORIENTED_EDGE ( 'NONE', *, *, #15981, .F. ) ;
#2486 = APPROVAL_DATE_TIME ( #15054, #20442 ) ;
#2487 = ORIENTED_EDGE ( 'NONE', *, *, #19919, .F. ) ;
#2488 = CARTESIAN_POINT ( 'NONE',  ( -7.000945310522701902E-17, 0.4446428569477722803, 0.3999999999999999667 ) ) ;
#2489 = CARTESIAN_POINT ( 'NONE',  ( -0.3070897238531018481, 5.003920639348050869, 0.05874023563891096061 ) ) ;
#2490 = ORIENTED_EDGE ( 'NONE', *, *, #15292, .T. ) ;
#2491 = CARTESIAN_POINT ( 'NONE',  ( -0.1167790944451422702, 0.1777777777019111383, -0.2819296736111110424 ) ) ;
#2492 = EDGE_LOOP ( 'NONE', ( #5141, #6398, #19661, #6485 ) ) ;
#2493 = CARTESIAN_POINT ( 'NONE',  ( 0.1948874010148183844, 0.4287475839277025136, 0.4171140917644197144 ) ) ;
#2494 = DIRECTION ( 'NONE',  ( -1.000000000000000000, 0.000000000000000000, 0.000000000000000000 ) ) ;
#2495 = CARTESIAN_POINT ( 'NONE',  ( 0.2923287055106771337, 0.1437499999024575981, -0.2123892367102620249 ) ) ;
#2496 = CARTESIAN_POINT ( 'NONE',  ( 0.1473522029762736330, 5.186493960802011749, -0.2512293203370171701 ) ) ;
#2497 = EDGE_LOOP ( 'NONE', ( #1375, #11890 ) ) ;
#2498 = CARTESIAN_POINT ( 'NONE',  ( -3.268767525105149064E-07, 3.877166675600695722, -0.3119999999998287477 ) ) ;
#2499 = CARTESIAN_POINT ( 'NONE',  ( -0.1144950937579609779, 0.2764156081756484196, 0.4668055555555604141 ) ) ;
#2500 = CIRCLE ( 'NONE', #13795, 0.2124999999999999944 ) ;
#2501 = CARTESIAN_POINT ( 'NONE',  ( -0.2819296736111110424, 4.023000000075866112, 0.1167790944451424923 ) ) ;
#2502 = CARTESIAN_POINT ( 'NONE',  ( -0.03226549977394326668, 0.03723082898989394512, 0.2853644822618193744 ) ) ;
#2503 = CARTESIAN_POINT ( 'NONE',  ( -0.1929987219779752405, 5.170199845349932488, -0.2252547127343075273 ) ) ;
#2504 = CARTESIAN_POINT ( 'NONE',  ( 0.2206173157302027954, 4.425777777929510215, -0.2206173157302028232 ) ) ;
#2505 = CARTESIAN_POINT ( 'NONE',  ( -0.1167790944451423535, 4.877166666742532186, 0.2819296736111110979 ) ) ;
#2506 = ORIENTED_EDGE ( 'NONE', *, *, #179, .T. ) ;
#2507 = CARTESIAN_POINT ( 'NONE',  ( 0.1993543840281267465, 4.040361111186976828, 0.1993543840281266633 ) ) ;
#2508 = ORIENTED_EDGE ( 'NONE', *, *, #3258, .T. ) ;
#2509 = ORIENTED_EDGE ( 'NONE', *, *, #4443, .F. ) ;
#2510 = ORIENTED_EDGE ( 'NONE', *, *, #6776, .F. ) ;
#2511 = APPROVAL_ROLE ( '' ) ;
#2512 = AXIS2_PLACEMENT_3D ( 'NONE', #7170, #1795, #18868 ) ;
#2513 = ORIENTED_EDGE ( 'NONE', *, *, #19139, .F. ) ;
#2514 = CARTESIAN_POINT ( 'NONE',  ( 0.4805453480892175055, 0.2624482906435715024, 0.04271891838947997760 ) ) ;
#2515 = FACE_OUTER_BOUND ( 'NONE', #12471, .T. ) ;
#2516 = CARTESIAN_POINT ( 'NONE',  ( 0.2206173157302028232, 0.07361111095937818150, -0.2206173157302028232 ) ) ;
#2517 = CARTESIAN_POINT ( 'NONE',  ( 0.06630425240443300894, 4.406804897824915024, 0.3048872720155125227 ) ) ;
#2518 = CARTESIAN_POINT ( 'NONE',  ( 0.000000000000000000, 0.3125000000000000000, 0.2758333333333368720 ) ) ;
#2519 = CARTESIAN_POINT ( 'NONE',  ( -0.3119999999999998885, 4.943138888888888083, 0.1292346314604058410 ) ) ;
#2520 = CARTESIAN_POINT ( 'NONE',  ( -0.2764156081756484196, -0.1144950937579609362, 0.1473611111111134409 ) ) ;
#2521 = CARTESIAN_POINT ( 'NONE',  ( -0.2819296736111110979, 0.5736111110352443143, -0.1167790944451423396 ) ) ;
#2522 = CARTESIAN_POINT ( 'NONE',  ( 0.1144950937579611444, 0.2764156081756483641, -0.09569444444444404063 ) ) ;
#2523 = EDGE_LOOP ( 'NONE', ( #17996, #19138, #13813, #19199 ) ) ;
#2524 = CARTESIAN_POINT ( 'NONE',  ( -0.1167790944451423257, 4.745222222298088433, -0.2819296736111110424 ) ) ;
#2525 = PLANE ( 'NONE',  #15932 ) ;
#2526 = CARTESIAN_POINT ( 'NONE',  ( 0.1167790944451422702, 4.613277777853643791, -0.2819296736111110424 ) ) ;
#2527 = CARTESIAN_POINT ( 'NONE',  ( 1.910449006669871087E-17, 0.3027777776260448528, -0.3119999999999999996 ) ) ;
#2528 = CARTESIAN_POINT ( 'NONE',  ( 0.2694814359950223892, 4.858521671012855592, 0.1585249534160457774 ) ) ;
#2529 = CARTESIAN_POINT ( 'NONE',  ( 1.573500000000000343, -3.414809992080329023E-17, -0.1400000000000000133 ) ) ;
#2530 = LINE ( 'NONE', #13753, #2649 ) ;
#2531 = CARTESIAN_POINT ( 'NONE',  ( 5.731347020009612645E-17, 4.175777777777776478, 0.3119999999999999996 ) ) ;
#2532 = CARTESIAN_POINT ( 'NONE',  ( -0.1292346314604056745, 5.213972222373953969, -0.3119999999999999996 ) ) ;
#2533 = AXIS2_PLACEMENT_3D ( 'NONE', #13434, #7334, #5741 ) ;
#2534 = CARTESIAN_POINT ( 'NONE',  ( 5.731347020009612645E-17, 4.009111111111109516, 0.3119999999999999996 ) ) ;
#2535 = VERTEX_POINT ( 'NONE', #17777 ) ;
#2536 = CARTESIAN_POINT ( 'NONE',  ( 0.08367912913462044466, 0.4929537096338479363, 0.07813342133392807420 ) ) ;
#2537 = VERTEX_POINT ( 'NONE', #23125 ) ;
#2538 = ORGANIZATION ( 'UNSPECIFIED', 'UNSPECIFIED', '' ) ;
#2539 = CARTESIAN_POINT ( 'NONE',  ( 0.09844450058468011411, 4.685553096116148453, 0.2967704092508852698 ) ) ;
#2540 = CARTESIAN_POINT ( 'NONE',  ( -0.1954553509668046640, 0.1954553509668046918, 0.3591666666666706864 ) ) ;
#2541 = AXIS2_PLACEMENT_3D ( 'NONE', #3708, #11515, #15740 ) ;
#2542 = CARTESIAN_POINT ( 'NONE',  ( 0.1572347947908322718, 4.316939703013657592, -0.2725648881498895504 ) ) ;
#2543 = ORIENTED_EDGE ( 'NONE', *, *, #2129, .F. ) ;
#2544 = CARTESIAN_POINT ( 'NONE',  ( -0.2233192592356399997, 0.04017857133102901990, 0.3073725909049499494 ) ) ;
#2545 = CARTESIAN_POINT ( 'NONE',  ( 1.726321361862525858E-17, 0.3826388888130222710, -0.2819296736111110979 ) ) ;
#2546 = CARTESIAN_POINT ( 'NONE',  ( 0.04084064317332824351, 3.850486187038780095, 0.3119999999999971685 ) ) ;
#2547 = DIRECTION ( 'NONE',  ( 0.000000000000000000, 0.000000000000000000, -1.000000000000000000 ) ) ;
#2548 = LINE ( 'NONE', #8502, #22219 ) ;
#2549 = CARTESIAN_POINT ( 'NONE',  ( -3.385114897866767815E-17, -0.2764156081756484196, 0.2758333333333366499 ) ) ;
#2550 = ORIENTED_EDGE ( 'NONE', *, *, #21102, .F. ) ;
#2551 = CARTESIAN_POINT ( 'NONE',  ( -0.1890277917641698391, 5.112901531185110926, 0.2452034757534968523 ) ) ;
#2552 = CC_DESIGN_PERSON_AND_ORGANIZATION_ASSIGNMENT ( #4508, #13790, ( #8363 ) ) ;
#2553 = CARTESIAN_POINT ( 'NONE',  ( 1.910449006669871087E-17, 0.1361111109593781676, -0.3119999999999999996 ) ) ;
#2554 = SECURITY_CLASSIFICATION ( '', '', #12634 ) ;
#2555 = CARTESIAN_POINT ( 'NONE',  ( 0.1292346314604070623, 4.734805555555555046, 0.3119999999999986673 ) ) ;
#2556 = CARTESIAN_POINT ( 'NONE',  ( -0.3119999999999999996, 0.2645833333333330040, -0.1292346314604056745 ) ) ;
#2557 = CARTESIAN_POINT ( 'NONE',  ( 0.2206173157302028787, 5.016055555555554157, 0.2206173157302027954 ) ) ;
#2558 = CARTESIAN_POINT ( 'NONE',  ( 0.1167790944451424368, 3.884111111186977272, 0.2819296736111110424 ) ) ;
#2559 = CARTESIAN_POINT ( 'NONE',  ( -1.910449006669871087E-17, 4.981333333333332725, -0.3119999999999999996 ) ) ;
#2560 = CARTESIAN_POINT ( 'NONE',  ( -0.1953806383670292079, 0.4284628132096496289, 0.4289620446068652670 ) ) ;
#2561 = CARTESIAN_POINT ( 'NONE',  ( 4.898587196589413075E-17, 3.700000000000000622, 0.4000000000000000222 ) ) ;
#2562 = ORIENTED_EDGE ( 'NONE', *, *, #20311, .T. ) ;
#2563 = CARTESIAN_POINT ( 'NONE',  ( -0.3125000000000010547, -0.1294417382415911644, 0.1265277777777800983 ) ) ;
#2564 = CARTESIAN_POINT ( 'NONE',  ( -0.2819296736111110424, 4.689666666742532186, 0.1167790944451424923 ) ) ;
#2565 = VECTOR ( 'NONE', #13692, 39.37007874015748143 ) ;
#2566 = CARTESIAN_POINT ( 'NONE',  ( 0.04626190099493247138, 0.5145565563726263170, 0.07046568677123667135 ) ) ;
#2567 = CARTESIAN_POINT ( 'NONE',  ( -0.3119999999999999996, 4.102861111111110404, -0.1292346314604056468 ) ) ;
#2568 = CARTESIAN_POINT ( 'NONE',  ( -0.4687500000000003886, 0.1725697052561470934, 0.06591547745735594488 ) ) ;
#2569 = CYLINDRICAL_SURFACE ( 'NONE', #16931, 0.2499999999999999722 ) ;
#2570 = LOCAL_TIME ( 21, 9, 13.00000000000000000, #8194 ) ;
#2571 = CARTESIAN_POINT ( 'NONE',  ( -0.1167790944451423535, 4.321611111186976828, 0.2819296736111110979 ) ) ;
#2572 = EDGE_CURVE ( 'NONE', #20446, #3858, #3522, .T. ) ;
#2573 = CARTESIAN_POINT ( 'NONE',  ( -0.1703658285323327304, 4.048932979482113836, -0.2616358941182676534 ) ) ;
#2574 = CARTESIAN_POINT ( 'NONE',  ( -3.385114897866767815E-17, -0.2764156081756484196, -0.001944444444443294917 ) ) ;
#2575 = CARTESIAN_POINT ( 'NONE',  ( -3.827021247335479543E-17, -0.3125000000000000000, 0.3591666666666709085 ) ) ;
#2576 = ORIENTED_EDGE ( 'NONE', *, *, #19990, .T. ) ;
#2577 = CLOSED_SHELL ( 'NONE', ( #12468, #17079, #9619, #12370, #1827, #20856, #11804, #20389, #18255 ) ) ;
#2578 = CARTESIAN_POINT ( 'NONE',  ( 0.2819296736111110424, 0.3861111110352444808, -0.1167790944451423119 ) ) ;
#2579 = CARTESIAN_POINT ( 'NONE',  ( 0.4620259694561523744, -0.2880908832651558615, 0.04413116910601658921 ) ) ;
#2580 = CARTESIAN_POINT ( 'NONE',  ( -0.1963547988595202021, 0.4279003813870556616, 0.09139143879391155301 ) ) ;
#2581 = AXIS2_PLACEMENT_3D ( 'NONE', #9693, #15302, #20664 ) ;
#2582 = DIRECTION ( 'NONE',  ( -0.000000000000000000, -1.000000000000000000, -0.000000000000000000 ) ) ;
#2583 = CARTESIAN_POINT ( 'NONE',  ( -0.3155070326520293400, 0.1306872919485614903, 0.1699305555555579161 ) ) ;
#2584 = ADVANCED_FACE ( 'NONE', ( #8501 ), #15825, .F. ) ;
#2585 = VERTEX_POINT ( 'NONE', #14003 ) ;
#2586 = CARTESIAN_POINT ( 'NONE',  ( 3.073863465859856523E-17, 0.4202679491924311006, -0.2510000000000000009 ) ) ;
#2587 = CARTESIAN_POINT ( 'NONE',  ( -0.3038758835458211238, 3.777719410249359200, -0.08167920987076236761 ) ) ;
#2588 = CARTESIAN_POINT ( 'NONE',  ( -0.1993543840281267465, 0.4034722221463555858, 0.1993543840281266633 ) ) ;
#2589 = CARTESIAN_POINT ( 'NONE',  ( 0.2819296736111110424, 0.1986111110352444253, 0.1167790944451424923 ) ) ;
#2590 = CARTESIAN_POINT ( 'NONE',  ( -0.2819296736111110979, 4.088972222298088433, 0.000000000000000000 ) ) ;
#2591 = CARTESIAN_POINT ( 'NONE',  ( 0.2472135954999579721, 0.2589285712334866152, -0.3402603233408159622 ) ) ;
#2592 = CARTESIAN_POINT ( 'NONE',  ( 0.2819296736111110979, 4.561194444520310753, -3.452642723725051716E-17 ) ) ;
#2593 = CARTESIAN_POINT ( 'NONE',  ( 0.000000000000000000, 2.735000000000000320, 0.7500000000000001110 ) ) ;
#2594 = CC_DESIGN_SECURITY_CLASSIFICATION ( #1033, ( #24136 ) ) ;
#2595 = ORIENTED_EDGE ( 'NONE', *, *, #8284, .F. ) ;
#2596 = CARTESIAN_POINT ( 'NONE',  ( -0.08337866210075467466, 0.4931271843567329172, 0.07807775719020894345 ) ) ;
#2597 = CARTESIAN_POINT ( 'NONE',  ( -0.2206173157302027676, 3.953555555707287894, 0.2206173157302028787 ) ) ;
#2598 = CARTESIAN_POINT ( 'NONE',  ( 0.1688124736067298515, -0.2196335248264128515, 0.3880822748423150559 ) ) ;
#2599 = AXIS2_PLACEMENT_3D ( 'NONE', #3199, #10645, #4783 ) ;
#2600 = ORIENTED_EDGE ( 'NONE', *, *, #11117, .F. ) ;
#2601 = EDGE_CURVE ( 'NONE', #6853, #13735, #12070, .T. ) ;
#2602 = ADVANCED_FACE ( 'NONE', ( #14121 ), #2628, .F. ) ;
#2603 = PERSON_AND_ORGANIZATION_ROLE ( 'design_supplier' ) ;
#2604 = CARTESIAN_POINT ( 'NONE',  ( -9.626299801968715084E-16, 0.3464285714285713635, -0.4000000000000000222 ) ) ;
#2605 =( BOUNDED_CURVE ( )  B_SPLINE_CURVE ( 2, ( #3662, #20131, #16597, #24017, #3786, #1600, #7327, #12717, #5369 ),
 .UNSPECIFIED., .F., .F. ) 
 B_SPLINE_CURVE_WITH_KNOTS ( ( 3, 2, 2, 2, 3 ),
 ( 0.1874999999999997224, 0.1919642857142855319, 0.1964285714285713413, 0.2008928571428571508, 0.2053571428571429325 ),
 .UNSPECIFIED. ) 
 CURVE ( )  GEOMETRIC_REPRESENTATION_ITEM ( )  RATIONAL_B_SPLINE_CURVE ( ( 1.000000000000004663, 0.9238795325112819645, 1.000000000000000000, 0.9238795325112867385, 1.000000000000000000, 0.9238795325112867385, 1.000000000000000000, 0.9238795325112852952, 1.000000000000001332 ) ) 
 REPRESENTATION_ITEM ( '' )  );
#2606 = CARTESIAN_POINT ( 'NONE',  ( -0.4516234456863258973, 1.487605717019675700, -2.675422173886249588 ) ) ;
#2607 = ORIENTED_EDGE ( 'NONE', *, *, #776, .T. ) ;
#2608 = CARTESIAN_POINT ( 'NONE',  ( -0.2819296736111110979, 0.1361111110352444808, 0.1167790944451422425 ) ) ;
#2609 = ORIENTED_EDGE ( 'NONE', *, *, #8677, .T. ) ;
#2610 = CARTESIAN_POINT ( 'NONE',  ( 0.2366305250842039298, 4.258541195428815485, -0.2048919769568291471 ) ) ;
#2611 = CARTESIAN_POINT ( 'NONE',  ( 0.3852690508742848685, 0.3188306871325746195, 0.4003899297375634325 ) ) ;
#2612 = CARTESIAN_POINT ( 'NONE',  ( 0.2779822102558559549, 4.089747752421554416, -0.1478112815533153268 ) ) ;
#2613 = CARTESIAN_POINT ( 'NONE',  ( 0.2923287055106771337, 0.3580357141881718164, -0.2123892367102620249 ) ) ;
#2614 = DIRECTION ( 'NONE',  ( 0.7071067811865476838, -0.7071067811865474617, 1.207317650931790858E-16 ) ) ;
#2615 = EDGE_CURVE ( 'NONE', #3437, #644, #21436, .T. ) ;
#2616 = CARTESIAN_POINT ( 'NONE',  ( -6.979263641208234666E-17, 0.4223214284738860402, 0.3799334167787516980 ) ) ;
#2617 = CARTESIAN_POINT ( 'NONE',  ( -0.4253970711649990855, -0.3089455473570085764, 0.05347937985141010958 ) ) ;
#2618 = CARTESIAN_POINT ( 'NONE',  ( -1.726321361862525858E-17, 4.061194444520309865, -0.2819296736111110979 ) ) ;
#2619 = CARTESIAN_POINT ( 'NONE',  ( -0.4251436100157495734, -0.2958090996784975002, 0.4013701042765217553 ) ) ;
#2620 = CARTESIAN_POINT ( 'NONE',  ( -0.1704140045665936964, 5.169151437939198956, -0.2432099552469337289 ) ) ;
#2621 = CARTESIAN_POINT ( 'NONE',  ( 0.3950000000000000178, 0.05000000000000028727, -1.966000000000000192 ) ) ;
#2622 = CARTESIAN_POINT ( 'NONE',  ( 0.1292346314604056190, 4.595916666818398610, -0.3119999999999999996 ) ) ;
#2623 = CARTESIAN_POINT ( 'NONE',  ( 0.1993543840281267465, 5.054250000075865223, 0.1993543840281266633 ) ) ;
#2624 = ORIENTED_EDGE ( 'NONE', *, *, #18763, .T. ) ;
#2625 = CARTESIAN_POINT ( 'NONE',  ( -0.2819296736111110424, 4.016055555631421470, -0.1167790944451423119 ) ) ;
#2626 = ORIENTED_EDGE ( 'NONE', *, *, #11276, .T. ) ;
#2627 = EDGE_CURVE ( 'NONE', #8315, #8144, #13936, .T. ) ;
#2628 = CONICAL_SURFACE ( 'NONE', #17417, 0.1874999999999998335, 1.029744258676652757 ) ;
#2629 = EDGE_LOOP ( 'NONE', ( #2985, #23303, #17357, #22746 ) ) ;
#2630 = APPROVAL_STATUS ( 'not_yet_approved' ) ;
#2631 = DIRECTION ( 'NONE',  ( -0.000000000000000000, -1.000000000000000000, -0.000000000000000000 ) ) ;
#2632 = CARTESIAN_POINT ( 'NONE',  ( -0.2206173157302028787, 0.1569444442927115102, 0.2206173157302027954 ) ) ;
#2633 = CARTESIAN_POINT ( 'NONE',  ( 0.2003325403190083509, 5.154788576413611878, -0.2249901030001114077 ) ) ;
#2634 = CARTESIAN_POINT ( 'NONE',  ( -0.4587627190187693049, 0.1786642205917136905, 0.4164153136193288751 ) ) ;
#2635 = DIRECTION ( 'NONE',  ( -0.4999999999999991673, -0.8660254037844391517, 0.000000000000000000 ) ) ;
#2636 = EDGE_CURVE ( 'NONE', #20833, #45, #8068, .T. ) ;
#2637 = CARTESIAN_POINT ( 'NONE',  ( 0.4224880990050952079, -0.2973422596752695601, 0.07046568677120454427 ) ) ;
#2638 = CARTESIAN_POINT ( 'NONE',  ( -0.1954553509668046640, 0.1954553509668046918, 0.2480555555555586933 ) ) ;
#2639 = CARTESIAN_POINT ( 'NONE',  ( -5.178964085587577574E-17, 0.07708333325746669074, 0.2819296736111110979 ) ) ;
#2640 = CARTESIAN_POINT ( 'NONE',  ( 0.1954553509668046640, -0.1954553509668047195, 0.1091666666666687158 ) ) ;
#2641 = ORIENTED_EDGE ( 'NONE', *, *, #3192, .F. ) ;
#2642 = CARTESIAN_POINT ( 'NONE',  ( 0.1993543840281266633, 4.679250000075866112, -0.1993543840281266910 ) ) ;
#2643 = DIRECTION ( 'NONE',  ( 0.4999999999999798495, 0.000000000000000000, -0.8660254037844501429 ) ) ;
#2644 = CARTESIAN_POINT ( 'NONE',  ( 0.1167790944451422702, 4.724388888964754507, -0.2819296736111110424 ) ) ;
#2645 = CARTESIAN_POINT ( 'NONE',  ( 0.1292346314604057300, 0.2784722220704892726, 0.3119999999999998885 ) ) ;
#2646 = CARTESIAN_POINT ( 'NONE',  ( -0.3150149228729092199, 0.4537208395564915620, -1.126438923088229904 ) ) ;
#2647 = FACE_OUTER_BOUND ( 'NONE', #2077, .T. ) ;
#2648 = CARTESIAN_POINT ( 'NONE',  ( -0.1292346314604056745, 4.262583333333332725, -0.3119999999999999996 ) ) ;
#2649 = VECTOR ( 'NONE', #21178, 39.37007874015748143 ) ;
#2650 = CARTESIAN_POINT ( 'NONE',  ( -0.1292346314604057023, 5.179250000151732536, 0.3119999999999998885 ) ) ;
#2651 = LINE ( 'NONE', #6663, #9593 ) ;
#2652 = VERTEX_POINT ( 'NONE', #12307 ) ;
#2653 = CARTESIAN_POINT ( 'NONE',  ( 0.000000000000000000, 0.000000000000000000, 0.2495000000000007212 ) ) ;
#2654 = EDGE_LOOP ( 'NONE', ( #12891, #3424, #4036, #22897, #22351, #12950 ) ) ;
#2655 = CARTESIAN_POINT ( 'NONE',  ( -0.3125000000000000000, 1.913510623667739771E-17, 0.06750000000000189182 ) ) ;
#2656 = APPLICATION_CONTEXT ( 'configuration controlled 3d designs of mechanical parts and assemblies' ) ;
#2657 = CARTESIAN_POINT ( 'NONE',  ( 0.2940001360523776808, 4.144101130514563636, -0.1069869603560802546 ) ) ;
#2658 = CARTESIAN_POINT ( 'NONE',  ( -3.863846776457871776E-17, -0.3155070326520292845, 0.07965277777777976520 ) ) ;
#2659 = VECTOR ( 'NONE', #20803, 39.37007874015748143 ) ;
#2660 = EDGE_CURVE ( 'NONE', #7579, #18699, #2777, .T. ) ;
#2661 = CARTESIAN_POINT ( 'NONE',  ( 5.731347020009612645E-17, 4.453555555555555046, 0.3119999999999999996 ) ) ;
#2662 = CARTESIAN_POINT ( 'NONE',  ( 0.3613381517857143232, -0.07767857152611380711, 0.000000000000000000 ) ) ;
#2663 = CARTESIAN_POINT ( 'NONE',  ( -0.09380593400082881672, 0.03242967361111052244, 0.2658661084243340578 ) ) ;
#2664 = CARTESIAN_POINT ( 'NONE',  ( -0.1144950937579609918, -0.2764156081756484196, -0.1165277777777775636 ) ) ;
#2665 = CARTESIAN_POINT ( 'NONE',  ( 0.8119709581221709049, 2.291712385858714729, -1.528283969076322801 ) ) ;
#2666 = DIRECTION ( 'NONE',  ( -0.000000000000000000, -1.000000000000000000, -0.000000000000000000 ) ) ;
#2667 = CARTESIAN_POINT ( 'NONE',  ( -0.1144950937579609779, 0.2764156081756484196, 0.3070833333333369275 ) ) ;
#2668 = EDGE_LOOP ( 'NONE', ( #22740, #19410 ) ) ;
#2669 = CARTESIAN_POINT ( 'NONE',  ( -0.2651997416066034785, 4.618152273832173194, 0.1652184020648941043 ) ) ;
#2670 = CARTESIAN_POINT ( 'NONE',  ( 1.573500000000000343, -3.414809992080329023E-17, -1.412500000000000089 ) ) ;
#2671 = CARTESIAN_POINT ( 'NONE',  ( 0.06791167322627879310, 1.376365001936863736E-16, -0.3730078252257436056 ) ) ;
#2672 = CARTESIAN_POINT ( 'NONE',  ( -0.3119999999999999996, 0.4937499999999996336, 0.1292346314604056190 ) ) ;
#2673 = CARTESIAN_POINT ( 'NONE',  ( 0.3119999999999999996, 4.908416666666665762, 0.1292346314604056190 ) ) ;
#2674 = CARTESIAN_POINT ( 'NONE',  ( -1.726321361862525858E-17, 4.019527777853643791, -0.2819296736111110979 ) ) ;
#2675 = DIRECTION ( 'NONE',  ( 0.000000000000000000, 0.000000000000000000, 1.000000000000000000 ) ) ;
#2676 = CARTESIAN_POINT ( 'NONE',  ( -0.2688280863486467442, 0.3751924628946938234, 0.4334272443489776694 ) ) ;
#2677 = CARTESIAN_POINT ( 'NONE',  ( 0.2994040877653771360, 1.697684548454547126E-17, 0.2026366584349470201 ) ) ;
#2678 = EDGE_LOOP ( 'NONE', ( #4352, #6182, #1396, #22973 ) ) ;
#2679 = ORIENTED_EDGE ( 'NONE', *, *, #19446, .T. ) ;
#2680 = VECTOR ( 'NONE', #18195, 39.37007874015748854 ) ;
#2681 = CARTESIAN_POINT ( 'NONE',  ( 0.1580000000000001403, -0.1079999999999998461, -1.920389328734020129 ) ) ;
#2682 = CARTESIAN_POINT ( 'NONE',  ( 0.1167790944451424368, 4.703555555631420582, 0.2819296736111110424 ) ) ;
#2683 = CARTESIAN_POINT ( 'NONE',  ( 0.3886629897678103296, -0.3298823763122805675, 0.06108558933789662304 ) ) ;
#2684 = CARTESIAN_POINT ( 'NONE',  ( -0.1754560956303653774, 5.162608100474836981, 0.2421305434278448743 ) ) ;
#2685 = CARTESIAN_POINT ( 'NONE',  ( -0.4687500000000003886, 0.2172233302825360146, 0.07046370559340160711 ) ) ;
#2686 = CC_DESIGN_PERSON_AND_ORGANIZATION_ASSIGNMENT ( #3463, #7009, ( #7006 ) ) ;
#2687 = CARTESIAN_POINT ( 'NONE',  ( 0.2764156081756484196, -5.077672346800151106E-17, -0.05055555555555477781 ) ) ;
#2688 = CARTESIAN_POINT ( 'NONE',  ( 0.2819296736111111534, 4.279944444520310753, 0.1167790944451422563 ) ) ;
#2689 = PERSON_AND_ORGANIZATION ( #7945, #5316 ) ;
#2690 = DIRECTION ( 'NONE',  ( 0.000000000000000000, -0.7071067811865376918, -0.7071067811865573427 ) ) ;
#2691 = CARTESIAN_POINT ( 'NONE',  ( 0.2764156081756483641, -0.1144950937579611028, 0.1195833333333354287 ) ) ;
#2692 = DIRECTION ( 'NONE',  ( 1.224646799147316476E-16, 0.000000000000000000, -1.000000000000000000 ) ) ;
#2693 = AXIS2_PLACEMENT_3D ( 'NONE', #3759, #16921, #783 ) ;
#2694 = CARTESIAN_POINT ( 'NONE',  ( 0.1993543840281266910, 0.4451388888130222710, -0.1993543840281266910 ) ) ;
#2695 = CARTESIAN_POINT ( 'NONE',  ( -1.910449006669871087E-17, 3.759111111111109960, -0.3119999999999999996 ) ) ;
#2696 = CARTESIAN_POINT ( 'NONE',  ( 1.845714884748260509, 0.000000000000000000, -2.498788568296995916 ) ) ;
#2697 = CARTESIAN_POINT ( 'NONE',  ( 0.1294417382415924134, 0.3124999999999999445, -0.01236111111111022273 ) ) ;
#2698 = CARTESIAN_POINT ( 'NONE',  ( 0.1306872919485616846, 0.3155070326520292290, 0.2115972222222248789 ) ) ;
#2699 = DIRECTION ( 'NONE',  ( -0.000000000000000000, -1.000000000000000000, -0.000000000000000000 ) ) ;
#2700 = CARTESIAN_POINT ( 'NONE',  ( -0.2726255772188902471, 3.784483688608106799, 0.1571220562871406545 ) ) ;
#2701 = CARTESIAN_POINT ( 'NONE',  ( -0.1993543840281267465, 0.5701388888130222155, 0.1993543840281266633 ) ) ;
#2702 = ADVANCED_FACE ( 'NONE', ( #17900 ), #22080, .T. ) ;
#2703 = CARTESIAN_POINT ( 'NONE',  ( 0.2819296736111110424, 0.4277777777019111105, -0.1167790944451423119 ) ) ;
#2704 = CARTESIAN_POINT ( 'NONE',  ( -0.1167790944451423535, 3.988277777853643347, 0.2819296736111110424 ) ) ;
#2705 = CARTESIAN_POINT ( 'NONE',  ( -0.1236067977499790416, 0.2982142855192009279, 0.3804226065180614236 ) ) ;
#2706 = CARTESIAN_POINT ( 'NONE',  ( 0.1167790944451422702, 4.627166666742533074, -0.2819296736111110424 ) ) ;
#2707 = CARTESIAN_POINT ( 'NONE',  ( 0.009375000000000067307, -0.5358532185916218271, 0.06112444011295370405 ) ) ;
#2708 = LINE ( 'NONE', #19772, #20370 ) ;
#2709 = VERTEX_POINT ( 'NONE', #17657 ) ;
#2710 = CARTESIAN_POINT ( 'NONE',  ( -1.910449006669871087E-17, 4.814666666666665762, -0.3119999999999999996 ) ) ;
#2711 = CARTESIAN_POINT ( 'NONE',  ( -0.2206173157302027676, 3.898000000151732092, 0.2206173157302028787 ) ) ;
#2712 = DIRECTION ( 'NONE',  ( -0.4995222938423280468, -0.04370253788966921987, 0.8651979924482607887 ) ) ;
#2713 = VECTOR ( 'NONE', #1717, 39.37007874015748143 ) ;
#2714 = CC_DESIGN_PERSON_AND_ORGANIZATION_ASSIGNMENT ( #2689, #17565, ( #15437 ) ) ;
#2715 = EDGE_CURVE ( 'NONE', #1184, #11161, #8627, .T. ) ;
#2716 = EDGE_LOOP ( 'NONE', ( #17071, #14816, #13647, #3130 ) ) ;
#2717 = PERSON_AND_ORGANIZATION_ROLE ( 'classification_officer' ) ;
#2718 = CARTESIAN_POINT ( 'NONE',  ( 9.101228903679513089E-16, 0.3107142857142856096, 0.4000000000000000222 ) ) ;
#2719 = CARTESIAN_POINT ( 'NONE',  ( -0.3071179979379754510, 4.559663454061065657, 0.06789499495992476485 ) ) ;
#2720 = ORIENTED_EDGE ( 'NONE', *, *, #14863, .F. ) ;
#2721 = CARTESIAN_POINT ( 'NONE',  ( -0.1993543840281267465, 0.02847222214635559273, 0.1993543840281266633 ) ) ;
#2722 = ORIENTED_EDGE ( 'NONE', *, *, #15876, .T. ) ;
#2723 = CARTESIAN_POINT ( 'NONE',  ( 0.01239007739188290914, 4.265721496431039483, -0.3117902882241837537 ) ) ;
#2724 = CARTESIAN_POINT ( 'NONE',  ( -0.2932070754709316107, 4.721180316163950508, -0.1095533496861972739 ) ) ;
#2725 = CARTESIAN_POINT ( 'NONE',  ( 0.3014967569398348535, 4.083227540263434818, 0.08027429777791007803 ) ) ;
#2726 = CARTESIAN_POINT ( 'NONE',  ( 0.2233192592356399164, 0.3401785713310290227, 0.3073725909049500604 ) ) ;
#2727 = CARTESIAN_POINT ( 'NONE',  ( 0.03846423745654679177, 5.168284486722195759, 0.2947504553715781239 ) ) ;
#2728 = AXIS2_PLACEMENT_3D ( 'NONE', #3771, #18642, #14511 ) ;
#2729 = CARTESIAN_POINT ( 'NONE',  ( -0.3613381517857143788, 0.3366071427596004084, 0.1174058825155740310 ) ) ;
#2730 = AXIS2_PLACEMENT_3D ( 'NONE', #5068, #5189, #1544 ) ;
#2731 = B_SPLINE_CURVE_WITH_KNOTS ( 'NONE', 3,
 ( #13951, #14305, #15773, #17719, #4669, #21739, #5024, #4551, #12014, #16255, #23667, #19426, #10178, #2724, #12138, #19545, #2837, #1014, #9050, #138, #1732, #9414, #12734, #11009, #16732, #18200, #13096, #22329 ),
 .UNSPECIFIED., .F., .F.,
 ( 4, 2, 2, 2, 2, 2, 2, 2, 2, 2, 2, 2, 2, 4 ),
 ( 0.3125972154215642673, 0.3141903899697943703, 0.3157835645180244732, 0.3173767390662545762, 0.3189699136144846792, 0.3205630881627147821, 0.3221562627109448851, 0.3237494372591749325, 0.3253426118074050355, 0.3269357863556351385, 0.3285289609038652414, 0.3317153100003254473, 0.3349016590967856533, 0.3380880081932458592 ),
 .UNSPECIFIED. ) ;
#2732 = CARTESIAN_POINT ( 'NONE',  ( 1.998815303304993796, 2.291712385858714285, -2.661240473580833488 ) ) ;
#2733 = CARTESIAN_POINT ( 'NONE',  ( -0.2819296736111110424, 3.849388888964754063, -0.1167790944451423119 ) ) ;
#2734 = CARTESIAN_POINT ( 'NONE',  ( 0.2827533054146886271, 5.033813457600698982, -0.1318886379381357665 ) ) ;
#2735 = CARTESIAN_POINT ( 'NONE',  ( -0.01917769073881700828, 5.163168389804723368, -0.2986873320831633927 ) ) ;
#2736 = FACE_OUTER_BOUND ( 'NONE', #9515, .T. ) ;
#2737 = CARTESIAN_POINT ( 'NONE',  ( -0.3119999999999998885, 4.505638889040620931, 0.1292346314604058410 ) ) ;
#2738 = CARTESIAN_POINT ( 'NONE',  ( -0.1993543840281266910, 4.748694444520309865, -0.1993543840281266910 ) ) ;
#2739 = VERTEX_POINT ( 'NONE', #13890 ) ;
#2740 = CARTESIAN_POINT ( 'NONE',  ( 0.1167790944451422702, 4.057722222298087544, -0.2819296736111110424 ) ) ;
#2741 = EDGE_CURVE ( 'NONE', #13618, #13239, #8261, .T. ) ;
#2742 = CONICAL_SURFACE ( 'NONE', #16383, 0.3125000000000000000, 0.7853981633974482790 ) ;
#2743 = VECTOR ( 'NONE', #4670, 39.37007874015748143 ) ;
#2744 = VERTEX_POINT ( 'NONE', #15593 ) ;
#2745 = APPROVAL_ROLE ( '' ) ;
#2746 = ORIENTED_EDGE ( 'NONE', *, *, #21858, .T. ) ;
#2747 = CARTESIAN_POINT ( 'NONE',  ( -0.03762146087705336983, -0.5076544266709852593, 0.4065068718547069637 ) ) ;
#2748 = CARTESIAN_POINT ( 'NONE',  ( -5.731347020009612645E-17, 0.2819444444444441089, 0.3119999999999999996 ) ) ;
#2749 = CARTESIAN_POINT ( 'NONE',  ( -0.3119999999999999996, 0.09444444429271151020, -3.820898013339742174E-17 ) ) ;
#2750 = CARTESIAN_POINT ( 'NONE',  ( 0.2634381141838555429, 5.151414792010848842, -0.1489582081906541955 ) ) ;
#2751 = CARTESIAN_POINT ( 'NONE',  ( -0.4687500000000003886, 0.2177858881633971400, 0.3900812861337792370 ) ) ;
#2752 = CARTESIAN_POINT ( 'NONE',  ( -0.4687500000000004996, -0.02206989609517173018, 0.4181409822411251698 ) ) ;
#2753 = LINE ( 'NONE', #19697, #2185 ) ;
#2754 = DIRECTION ( 'NONE',  ( 0.000000000000000000, 1.000000000000000000, 0.000000000000000000 ) ) ;
#2755 = CARTESIAN_POINT ( 'NONE',  ( -0.2764156081756484196, -0.1144950937579609362, 0.09180555555555744429 ) ) ;
#2756 = EDGE_LOOP ( 'NONE', ( #11888, #10367 ) ) ;
#2757 = DIRECTION ( 'NONE',  ( -0.000000000000000000, -1.000000000000000000, -0.000000000000000000 ) ) ;
#2758 = CARTESIAN_POINT ( 'NONE',  ( 0.1993543840281267465, 4.373694444520309865, 0.1993543840281266633 ) ) ;
#2759 = CARTESIAN_POINT ( 'NONE',  ( 0.2705345477997488368, 0.1189582700827290229, -0.08454861231499928576 ) ) ;
#2760 = LINE ( 'NONE', #8356, #1981 ) ;
#2761 = CARTESIAN_POINT ( 'NONE',  ( -0.2977100099089716734, 3.700000000000000622, 0.09499999999999995948 ) ) ;
#2762 = CARTESIAN_POINT ( 'NONE',  ( 0.1292346314604057300, 0.4451388887371560132, 0.3119999999999998885 ) ) ;
#2763 = CARTESIAN_POINT ( 'NONE',  ( -1.910449006669871087E-17, 4.370222222222221120, -0.3119999999999999996 ) ) ;
#2764 = EDGE_CURVE ( 'NONE', #13263, #22290, #20047, .T. ) ;
#2765 = CARTESIAN_POINT ( 'NONE',  ( 0.2098724675597480049, 4.981782548361976204, -0.2345071763989569069 ) ) ;
#2766 = DIRECTION ( 'NONE',  ( 0.000000000000000000, 0.000000000000000000, -1.000000000000000000 ) ) ;
#2767 = EDGE_CURVE ( 'NONE', #22988, #16899, #19073, .T. ) ;
#2768 = CARTESIAN_POINT ( 'NONE',  ( 0.03691426518906104626, 4.709496014152167120, -0.3099139152953400700 ) ) ;
#2769 = ORIENTED_EDGE ( 'NONE', *, *, #17414, .T. ) ;
#2770 = CARTESIAN_POINT ( 'NONE',  ( -0.2230971623002953874, 0.2230971623002954152, -0.05229166666666570235 ) ) ;
#2771 = AXIS2_PLACEMENT_3D ( 'NONE', #18468, #22241, #5662 ) ;
#2772 = DIRECTION ( 'NONE',  ( -0.000000000000000000, -1.000000000000000000, -0.000000000000000000 ) ) ;
#2773 = ORIENTED_EDGE ( 'NONE', *, *, #10048, .T. ) ;
#2774 = CARTESIAN_POINT ( 'NONE',  ( 0.2233192592356399997, 0.2901785713310290338, -0.3073725909049500049 ) ) ;
#2775 = CARTESIAN_POINT ( 'NONE',  ( -0.1167790944451422702, 0.06666666659080003332, -0.2819296736111110979 ) ) ;
#2776 = CARTESIAN_POINT ( 'NONE',  ( 0.1954553509668047195, 0.1954553509668046085, 0.1300000000000021694 ) ) ;
#2777 = LINE ( 'NONE', #10471, #10819 ) ;
#2778 = DIRECTION ( 'NONE',  ( 0.000000000000000000, 0.000000000000000000, -1.000000000000000000 ) ) ;
#2779 = CARTESIAN_POINT ( 'NONE',  ( 0.2764156081756484196, -5.077672346800151106E-17, 0.4563888888888936735 ) ) ;
#2780 = VERTEX_POINT ( 'NONE', #8207 ) ;
#2781 = CARTESIAN_POINT ( 'NONE',  ( -0.1094414729302275041, 5.115363257335545200, 0.2892685870146211591 ) ) ;
#2782 = CARTESIAN_POINT ( 'NONE',  ( 0.3236067977499790249, 0.1214285714285713996, -0.2351141009169892826 ) ) ;
#2783 = CYLINDRICAL_SURFACE ( 'NONE', #17237, 0.3119999999999999996 ) ;
#2784 = CARTESIAN_POINT ( 'NONE',  ( 0.3119999999999999996, 0.5770833333333330595, -0.1292346314604056468 ) ) ;
#2785 = CARTESIAN_POINT ( 'NONE',  ( -0.1292346314604057023, 4.950083333333331836, 0.3119999999999998885 ) ) ;
#2786 = CARTESIAN_POINT ( 'NONE',  ( -0.2819296736111110979, 4.238277777853642903, -0.1167790944451422980 ) ) ;
#2787 = CARTESIAN_POINT ( 'NONE',  ( -1.726321361862525858E-17, 3.963972222298087988, -0.2819296736111110979 ) ) ;
#2788 = DIRECTION ( 'NONE',  ( 1.000000000000000000, 0.000000000000000000, 0.000000000000000000 ) ) ;
#2789 = CARTESIAN_POINT ( 'NONE',  ( -0.2732891327808207316, 0.3834823229876400674, 0.4280258002685754515 ) ) ;
#2790 = CARTESIAN_POINT ( 'NONE',  ( 0.1437411428072669917, 4.817336466253104632, -0.2795564064785391878 ) ) ;
#2791 = VERTEX_POINT ( 'NONE', #2498 ) ;
#2792 = ORIENTED_EDGE ( 'NONE', *, *, #8595, .T. ) ;
#2793 = CARTESIAN_POINT ( 'NONE',  ( -0.2209708691207961095, 0.2209708691207961373, 0.1161111111111133992 ) ) ;
#2794 = CARTESIAN_POINT ( 'NONE',  ( -0.1167790944451423257, 4.620222222298087544, -0.2819296736111110424 ) ) ;
#2795 = FACE_OUTER_BOUND ( 'NONE', #17143, .T. ) ;
#2796 = CARTESIAN_POINT ( 'NONE',  ( -0.02386323619205392085, 4.515404379429468484, 0.3110906963637425360 ) ) ;
#2797 = PERSON_AND_ORGANIZATION_ROLE ( 'design_owner' ) ;
#2798 = CARTESIAN_POINT ( 'NONE',  ( 0.2111984196243031631, 0.4085062965502690990, 0.4344098397133764333 ) ) ;
#2799 = CARTESIAN_POINT ( 'NONE',  ( -3.385114897866767815E-17, -0.2764156081756484196, -0.06444444444444379083 ) ) ;
#2800 = CARTESIAN_POINT ( 'NONE',  ( 0.2819296736111110979, 4.005638888964754507, -3.452642723725051716E-17 ) ) ;
#2801 = ITEM_DEFINED_TRANSFORMATION ( 'NONE', 'NONE', #13069,  #9127 ) ;
#2802 = CARTESIAN_POINT ( 'NONE',  ( -0.2209708691207961095, 0.2209708691207961373, -0.05749999999999948208 ) ) ;
#2803 = DIRECTION ( 'NONE',  ( -0.000000000000000000, -1.000000000000000000, -0.000000000000000000 ) ) ;
#2804 = CARTESIAN_POINT ( 'NONE',  ( 0.2764156081756483641, 0.1144950937579610195, 0.1820833333333359005 ) ) ;
#2805 = CARTESIAN_POINT ( 'NONE',  ( 0.3236067977499790249, 0.2642857142857141795, -0.2351141009169892826 ) ) ;
#2806 = CARTESIAN_POINT ( 'NONE',  ( -0.1993543840281266633, 0.1118055554796889145, -0.1993543840281266910 ) ) ;
#2807 = CARTESIAN_POINT ( 'NONE',  ( 0.4687500000000002776, -0.04363837962608485554, 0.07944711129966139374 ) ) ;
#2808 = CARTESIAN_POINT ( 'NONE',  ( -0.2206173157302028787, 0.4416666666666662633, 0.2206173157302027954 ) ) ;
#2809 = CARTESIAN_POINT ( 'NONE',  ( -1.910449006669871087E-17, 3.925777777777776922, -0.3119999999999999996 ) ) ;
#2810 = CARTESIAN_POINT ( 'NONE',  ( 8.984713656453739555E-13, 5.162518060853549251, -0.2988821118451543968 ) ) ;
#2811 = CARTESIAN_POINT ( 'NONE',  ( -0.3155070326520292845, 1.931923388228935888E-17, 0.3400694444444480879 ) ) ;
#2812 = ORIENTED_EDGE ( 'NONE', *, *, #2339, .T. ) ;
#2813 = CARTESIAN_POINT ( 'NONE',  ( 0.2206173157302027954, 3.974388888888888083, -0.2206173157302028232 ) ) ;
#2814 = CARTESIAN_POINT ( 'NONE',  ( -0.1319936186941939871, 0.1819936186941943090, -0.5389016700558214579 ) ) ;
#2815 = CARTESIAN_POINT ( 'NONE',  ( -0.08166012297515250207, 3.823835601340495494, -0.3038808721544720148 ) ) ;
#2816 = CARTESIAN_POINT ( 'NONE',  ( -0.2819296736111110424, 0.5041666665908000056, -0.1167790944451423396 ) ) ;
#2817 = CARTESIAN_POINT ( 'NONE',  ( -0.1993543840281266355, 4.095916666742533074, 0.1993543840281267465 ) ) ;
#2818 = CARTESIAN_POINT ( 'NONE',  ( 2.326421213736078119E-17, 0.02946428561674332286, -0.3799334167787516425 ) ) ;
#2819 = VECTOR ( 'NONE', #22880, 39.37007874015748143 ) ;
#2820 = CARTESIAN_POINT ( 'NONE',  ( 0.2819296736111110979, 4.616750000075865223, -3.452642723725051716E-17 ) ) ;
#2821 = CARTESIAN_POINT ( 'NONE',  ( 0.2908167028465252213, 5.128327494763021299, 0.1005549492768820219 ) ) ;
#2822 = CARTESIAN_POINT ( 'NONE',  ( 0.1864859647049422198, 5.086573399267850348, -0.2501715381927130388 ) ) ;
#2823 = VERTEX_POINT ( 'NONE', #9937 ) ;
#2824 = ORIENTED_EDGE ( 'NONE', *, *, #9965, .F. ) ;
#2825 = PLANE ( 'NONE',  #6205 ) ;
#2826 = CARTESIAN_POINT ( 'NONE',  ( 0.3119999999999999996, 3.748694444596176734, 0.1292346314604056190 ) ) ;
#2827 = DIRECTION ( 'NONE',  ( 0.4999999999999913403, 0.000000000000000000, -0.8660254037844434816 ) ) ;
#2828 = ORIENTED_EDGE ( 'NONE', *, *, #19144, .F. ) ;
#2829 = SHAPE_DEFINITION_REPRESENTATION ( #3106, #20236 ) ;
#2830 = AXIS2_PLACEMENT_3D ( 'NONE', #7328, #6846, #14654 ) ;
#2831 = CARTESIAN_POINT ( 'NONE',  ( -0.4687500000000004441, 0.2570931668155772565, 0.04874733047933996199 ) ) ;
#2832 = CARTESIAN_POINT ( 'NONE',  ( -0.2450385544630677703, 4.551749392525340276, -0.1971986354532856700 ) ) ;
#2833 = VERTEX_POINT ( 'NONE', #17368 ) ;
#2834 = CARTESIAN_POINT ( 'NONE',  ( 1.726321361862525858E-17, 0.007638888813022257952, -0.2819296736111110979 ) ) ;
#2835 = CARTESIAN_POINT ( 'NONE',  ( 0.2819296736111110424, 0.1013888888130222432, 0.1167790944451424923 ) ) ;
#2836 = EDGE_CURVE ( 'NONE', #10294, #22559, #3402, .T. ) ;
#2837 = CARTESIAN_POINT ( 'NONE',  ( -0.2490186137998644522, 4.718604494521838610, -0.1890786097946130784 ) ) ;
#2838 = CARTESIAN_POINT ( 'NONE',  ( 0.3072473562388144397, 4.087380897120025836, -0.06871205321792885068 ) ) ;
#2839 = CARTESIAN_POINT ( 'NONE',  ( 0.1116596296178199860, 0.3651785713310289894, -0.3436530038418508792 ) ) ;
#2840 = CARTESIAN_POINT ( 'NONE',  ( -0.2206173157302028232, 4.488277777777776478, -0.2206173157302028232 ) ) ;
#2841 = DIRECTION ( 'NONE',  ( 0.000000000000000000, 0.000000000000000000, 1.000000000000000000 ) ) ;
#2842 = CYLINDRICAL_SURFACE ( 'NONE', #21055, 0.3125000000000000000 ) ;
#2843 = CARTESIAN_POINT ( 'NONE',  ( 0.1993543840281266633, 3.887583333409198705, -0.1993543840281266910 ) ) ;
#2844 = APPROVAL ( #14140, 'UNSPECIFIED' ) ;
#2845 = CARTESIAN_POINT ( 'NONE',  ( 0.1553973393617723575, 5.020657948710086416, 0.2736341191248760629 ) ) ;
#2846 = DIRECTION ( 'NONE',  ( -0.000000000000000000, 1.000000000000000000, -0.000000000000000000 ) ) ;
#2847 = CARTESIAN_POINT ( 'NONE',  ( 2.936000000000000387, 0.04999999999999970440, -2.591000000000000636 ) ) ;
#2848 = CARTESIAN_POINT ( 'NONE',  ( -0.3119999999999999996, 4.557722222373954857, 0.000000000000000000 ) ) ;
#2849 = AXIS2_PLACEMENT_3D ( 'NONE', #1084, #605, #957 ) ;
#2850 = CARTESIAN_POINT ( 'NONE',  ( -0.1993543840281266910, 4.637583333409199149, -0.1993543840281266910 ) ) ;
#2851 = VERTEX_POINT ( 'NONE', #16138 ) ;
#2852 = CARTESIAN_POINT ( 'NONE',  ( 0.2819296736111110424, 4.106333333409199149, -0.1167790944451423396 ) ) ;
#2853 = EDGE_LOOP ( 'NONE', ( #10665, #14476, #21486, #12136, #16151 ) ) ;
#2854 = ORIENTED_EDGE ( 'NONE', *, *, #21097, .F. ) ;
#2855 = DATE_AND_TIME ( #10195, #16569 ) ;
#2856 = CARTESIAN_POINT ( 'NONE',  ( 0.4692112248683192322, 0.2611554184491500785, 0.04763613967037012842 ) ) ;
#2857 = CARTESIAN_POINT ( 'NONE',  ( 0.3119999999999999996, 0.4624999999999996336, 0.000000000000000000 ) ) ;
#2858 = CARTESIAN_POINT ( 'NONE',  ( 0.3119999999999999996, 0.1222222220704892864, 0.000000000000000000 ) ) ;
#2859 = CARTESIAN_POINT ( 'NONE',  ( -1.493307031895086562E-17, 0.4842666352810564567, -1.161472000792705517 ) ) ;
#2860 = ADVANCED_FACE ( 'NONE', ( #10652 ), #1141, .T. ) ;
#2861 = FACE_OUTER_BOUND ( 'NONE', #4905, .T. ) ;
#2862 = CARTESIAN_POINT ( 'NONE',  ( 0.02812428215829835404, 0.1573150382780598433, -0.7495055110531126941 ) ) ;
#2863 = VERTEX_POINT ( 'NONE', #4787 ) ;
#2864 = EDGE_LOOP ( 'NONE', ( #15028, #19768, #5292, #18193 ) ) ;
#2865 = CARTESIAN_POINT ( 'NONE',  ( 0.1292346314604056745, 0.2437499998482670904, -0.3119999999999999996 ) ) ;
#2866 = FACE_OUTER_BOUND ( 'NONE', #22246, .T. ) ;
#2867 = CARTESIAN_POINT ( 'NONE',  ( -0.1144950937579609779, 0.2764156081756484196, -0.03319444444444354797 ) ) ;
#2868 = DIRECTION ( 'NONE',  ( -0.5773502691896257311, -0.5773502691896257311, 0.5773502691896257311 ) ) ;
#2869 = EDGE_CURVE ( 'NONE', #20123, #1184, #16017, .T. ) ;
#2870 = CARTESIAN_POINT ( 'NONE',  ( 0.1167790944451422702, 4.335500000075866112, -0.2819296736111110424 ) ) ;
#2871 = CARTESIAN_POINT ( 'NONE',  ( -0.01197057051269659507, 0.2890469299669656822, -0.07784597376562178705 ) ) ;
#2872 = CARTESIAN_POINT ( 'NONE',  ( -0.2825450144231913541, 0.3409525236117377789, -1.166144907693487776 ) ) ;
#2873 = PLANE ( 'NONE',  #2465 ) ;
#2874 = CARTESIAN_POINT ( 'NONE',  ( 0.4449999999999992295, 3.150471934781994425E-18, -0.04999999999999917705 ) ) ;
#2875 = CARTESIAN_POINT ( 'NONE',  ( 0.2206173157302028787, 4.349388888888888083, 0.2206173157302027954 ) ) ;
#2876 = CARTESIAN_POINT ( 'NONE',  ( 0.1292346314604056190, 5.207027777929509327, -0.3119999999999999996 ) ) ;
#2877 = CARTESIAN_POINT ( 'NONE',  ( 0.04104138843526779906, 4.961624887611388424, 0.3099691146773075334 ) ) ;
#2878 = ORIENTED_EDGE ( 'NONE', *, *, #646, .T. ) ;
#2879 = PLANE ( 'NONE',  #14029 ) ;
#2880 = EDGE_LOOP ( 'NONE', ( #14907, #2508, #5004, #8927 ) ) ;
#2881 = AXIS2_PLACEMENT_3D ( 'NONE', #84, #7650, #5814 ) ;
#2882 = CARTESIAN_POINT ( 'NONE',  ( 0.01963551970466389379, 4.683222298665006278, 0.3115337314451123718 ) ) ;
#2883 = CARTESIAN_POINT ( 'NONE',  ( 0.2540558108961654682, 4.146614437982985457, -0.1864098413859918979 ) ) ;
#2884 = CARTESIAN_POINT ( 'NONE',  ( 0.2230971623002953874, -0.2230971623002954429, -0.02451388888888771794 ) ) ;
#2885 = CARTESIAN_POINT ( 'NONE',  ( -0.1116596296178199582, 0.3901785713310289561, -0.3436530038418508792 ) ) ;
#2886 =( GEOMETRIC_REPRESENTATION_CONTEXT ( 3 ) GLOBAL_UNCERTAINTY_ASSIGNED_CONTEXT ( ( #22892 ) ) GLOBAL_UNIT_ASSIGNED_CONTEXT ( ( #6246, #15523, #8191 ) ) REPRESENTATION_CONTEXT ( 'NONE', 'WORKASPACE' ) );
#2887 = EDGE_CURVE ( 'NONE', #2585, #6063, #18083, .T. ) ;
#2888 = EDGE_CURVE ( 'NONE', #549, #22264, #8449, .T. ) ;
#2889 = CARTESIAN_POINT ( 'NONE',  ( 0.000000000000000000, 5.384999999999999787, 0.000000000000000000 ) ) ;
#2890 = CARTESIAN_POINT ( 'NONE',  ( -0.3613381517857144343, 0.3187499999024576147, 0.1174058825155740171 ) ) ;
#2891 = CARTESIAN_POINT ( 'NONE',  ( 0.2819296736111110979, 0.1048611110352444808, 0.000000000000000000 ) ) ;
#2892 = CARTESIAN_POINT ( 'NONE',  ( -3.385114897866767815E-17, -0.2764156081756484196, -0.05749999999999930167 ) ) ;
#2893 = DIRECTION ( 'NONE',  ( -1.000000000000000000, 0.000000000000000000, 0.000000000000000000 ) ) ;
#2894 = CARTESIAN_POINT ( 'NONE',  ( 0.2209708691207961095, -0.2209708691207961651, 0.08138888888889052320 ) ) ;
#2895 = CARTESIAN_POINT ( 'NONE',  ( -0.1144950937579609918, -0.2764156081756484196, 0.3834722222222265442 ) ) ;
#2896 = CIRCLE ( 'NONE', #12673, 0.7199999999999994182 ) ;
#2897 = EDGE_CURVE ( 'NONE', #17212, #9355, #18589, .T. ) ;
#2898 = ORIENTED_EDGE ( 'NONE', *, *, #23620, .T. ) ;
#2899 = CARTESIAN_POINT ( 'NONE',  ( 3.827021247335479543E-17, 5.500232050807569273, 0.3125000000000001665 ) ) ;
#2900 = CARTESIAN_POINT ( 'NONE',  ( -0.2574330024693365915, 4.274579109818574807, -0.1777445644304753436 ) ) ;
#2901 = FACE_OUTER_BOUND ( 'NONE', #21876, .T. ) ;
#2902 = CARTESIAN_POINT ( 'NONE',  ( 0.3119999999999998885, 0.5145833333333330595, 0.1292346314604058410 ) ) ;
#2903 = CARTESIAN_POINT ( 'NONE',  ( -1.910449006669871087E-17, 4.981333333333332725, -0.3119999999999999996 ) ) ;
#2904 = CARTESIAN_POINT ( 'NONE',  ( 0.2819296736111110979, 4.161888888964754507, -0.1167790944451423396 ) ) ;
#2905 = CARTESIAN_POINT ( 'NONE',  ( 0.2819296736111110424, 3.953555555631421914, -0.1167790944451423396 ) ) ;
#2906 = CARTESIAN_POINT ( 'NONE',  ( -0.4500000000000003997, -0.2598076211353319009, 0.3779506566538942125 ) ) ;
#2907 = DIRECTION ( 'NONE',  ( 0.000000000000000000, 0.000000000000000000, 1.000000000000000000 ) ) ;
#2908 = CARTESIAN_POINT ( 'NONE',  ( 0.3110098031160312138, 4.807043492563579434, 0.02485275949016588215 ) ) ;
#2909 = LOCAL_TIME ( 21, 9, 13.00000000000000000, #6094 ) ;
#2910 = ORIENTED_EDGE ( 'NONE', *, *, #10241, .F. ) ;
#2911 = ORIENTED_EDGE ( 'NONE', *, *, #8092, .F. ) ;
#2912 = CARTESIAN_POINT ( 'NONE',  ( -0.04087474790194534774, 3.989444776327029096, -0.3120000000000006657 ) ) ;
#2913 = CARTESIAN_POINT ( 'NONE',  ( 5.178964085587577574E-17, 4.422305555631421470, 0.2819296736111110979 ) ) ;
#2914 = CARTESIAN_POINT ( 'NONE',  ( 0.1567390680359450617, -0.2674066423994601593, 0.4211701672829530896 ) ) ;
#2915 = EDGE_CURVE ( 'NONE', #23447, #12633, #19670, .T. ) ;
#2916 = CARTESIAN_POINT ( 'NONE',  ( -0.2608208652903403757, 4.496968897623760064, -0.1766640260429742371 ) ) ;
#2917 = CIRCLE ( 'NONE', #12691, 1.200750000000023521 ) ;
#2918 = DATE_TIME_ROLE ( 'classification_date' ) ;
#2919 = CARTESIAN_POINT ( 'NONE',  ( -0.4805070082343984583, 0.2560807851245828215, 0.04413116910601664472 ) ) ;
#2920 = CARTESIAN_POINT ( 'NONE',  ( -0.2764156081756484196, 0.1144950937579609918, -0.02624999999999903799 ) ) ;
#2921 = CARTESIAN_POINT ( 'NONE',  ( -0.1167790944451423535, 3.988277777853643347, 0.2819296736111110979 ) ) ;
#2922 = LINE ( 'NONE', #23509, #16179 ) ;
#2923 = CARTESIAN_POINT ( 'NONE',  ( 0.000000000000000000, 6.000000000000000888, -0.2041999999999999926 ) ) ;
#2924 =( BOUNDED_CURVE ( )  B_SPLINE_CURVE ( 2, ( #12500, #12863, #4494, #8268, #15481, #20843, #22789, #2555, #10002 ),
 .UNSPECIFIED., .F., .T. ) 
 B_SPLINE_CURVE_WITH_KNOTS ( ( 3, 2, 2, 2, 3 ),
 ( 0.3303571428571427937, 0.3348214285714284921, 0.3392857142857142461, 0.3437499999999999445, 0.3482142857142856429 ),
 .UNSPECIFIED. ) 
 CURVE ( )  GEOMETRIC_REPRESENTATION_ITEM ( )  RATIONAL_B_SPLINE_CURVE ( ( 1.000000000000000888, 0.9238795325112857393, 1.000000000000000000, 0.9238795325112867385, 1.000000000000000000, 0.9238795325112867385, 1.000000000000000000, 0.9238795325112877377, 0.9999999999999990008 ) ) 
 REPRESENTATION_ITEM ( '' )  );
#2925 = CARTESIAN_POINT ( 'NONE',  ( -0.1144950937579609918, -0.2764156081756484196, 0.1612500000000024192 ) ) ;
#2926 = SECURITY_CLASSIFICATION ( '', '', #9805 ) ;
#2927 = CARTESIAN_POINT ( 'NONE',  ( 0.3613381517857143232, 0.1544642856167432743, 0.000000000000000000 ) ) ;
#2928 = B_SPLINE_CURVE_WITH_KNOTS ( 'NONE', 3,
 ( #6318, #17778, #19601, #15594, #9996, #21319 ),
 .UNSPECIFIED., .F., .F.,
 ( 4, 2, 4 ),
 ( 0.000000000000000000, 0.0002551367231383054666, 0.0005102734462766109333 ),
 .UNSPECIFIED. ) ;
#2929 = CARTESIAN_POINT ( 'NONE',  ( 0.1993543840281266355, 0.08402777770191115214, 0.1993543840281267465 ) ) ;
#2930 = CARTESIAN_POINT ( 'NONE',  ( -0.2365780681204351643, 0.1757304751630116846, 0.4057683715178541650 ) ) ;
#2931 = CARTESIAN_POINT ( 'NONE',  ( 0.4805070082343983473, 0.2560807851245830991, 0.04413116910601658921 ) ) ;
#2932 = CARTESIAN_POINT ( 'NONE',  ( 0.000000000000000000, 6.000000000000000888, 0.000000000000000000 ) ) ;
#2933 = CARTESIAN_POINT ( 'NONE',  ( -0.1236067977499790416, 0.3785714285714284477, 0.3804226065180614236 ) ) ;
#2934 = CARTESIAN_POINT ( 'NONE',  ( -0.2230971623002954152, -0.2230971623002953874, 0.3470138888888926187 ) ) ;
#2935 = EDGE_LOOP ( 'NONE', ( #4577, #11659, #9443, #16326 ) ) ;
#2936 = LINE ( 'NONE', #5115, #22346 ) ;
#2937 = DIRECTION ( 'NONE',  ( 0.000000000000000000, -0.7071067811865474617, 0.7071067811865474617 ) ) ;
#2938 = DIRECTION ( 'NONE',  ( 0.000000000000000000, 1.000000000000000000, 0.000000000000000000 ) ) ;
#2939 = CARTESIAN_POINT ( 'NONE',  ( -0.2819296736111110979, 0.3965277777019111660, -3.452642723725051716E-17 ) ) ;
#2940 = CARTESIAN_POINT ( 'NONE',  ( -0.1167790944451423257, 4.023000000075866112, -0.2819296736111110424 ) ) ;
#2941 = CARTESIAN_POINT ( 'NONE',  ( 0.3999999999999999667, 0.4589285712334866263, 0.1299678784931626307 ) ) ;
#2942 = VECTOR ( 'NONE', #1534, 39.37007874015748143 ) ;
#2943 = EDGE_LOOP ( 'NONE', ( #20914, #21292, #523, #8389 ) ) ;
#2944 = CARTESIAN_POINT ( 'NONE',  ( -1.726321361862525858E-17, 4.686194444520309865, -0.2819296736111110979 ) ) ;
#2945 = CARTESIAN_POINT ( 'NONE',  ( 0.2905596657203107225, 5.133515633311446003, -0.09673461593479984466 ) ) ;
#2946 = LINE ( 'NONE', #12236, #3236 ) ;
#2947 = ORIENTED_EDGE ( 'NONE', *, *, #1578, .F. ) ;
#2948 = CARTESIAN_POINT ( 'NONE',  ( 2.986000000000000210, 0.05000000000000028727, 0.000000000000000000 ) ) ;
#2949 = CARTESIAN_POINT ( 'NONE',  ( 0.2819296736111110979, 5.099388888964754507, 0.1167790944451422425 ) ) ;
#2950 = APPROVAL_PERSON_ORGANIZATION ( #1157, #15656, #14933 ) ;
#2951 = CARTESIAN_POINT ( 'NONE',  ( -9.626299801968715084E-16, 0.2660714283763437327, -0.4000000000000000222 ) ) ;
#2952 = ORIENTED_EDGE ( 'NONE', *, *, #11723, .T. ) ;
#2953 = CONICAL_SURFACE ( 'NONE', #17749, 0.3125000000000000000, 0.7853981633974482790 ) ;
#2954 = CARTESIAN_POINT ( 'NONE',  ( 0.2819296736111110979, 4.995222222298087544, -0.1167790944451423396 ) ) ;
#2955 = PERSON_AND_ORGANIZATION_ROLE ( 'design_supplier' ) ;
#2956 = ORIENTED_EDGE ( 'NONE', *, *, #21533, .T. ) ;
#2957 = CARTESIAN_POINT ( 'NONE',  ( -0.2040850575673537060, 5.106812889253229848, -0.2344380848128326533 ) ) ;
#2958 = CARTESIAN_POINT ( 'NONE',  ( 0.2206173157302027676, 0.2333333333333330040, 0.2206173157302028787 ) ) ;
#2959 = ORIENTED_EDGE ( 'NONE', *, *, #9659, .T. ) ;
#2960 = CARTESIAN_POINT ( 'NONE',  ( 0.1993543840281266355, 0.3756944443685777957, 0.1993543840281267465 ) ) ;
#2961 = VERTEX_POINT ( 'NONE', #15778 ) ;
#2962 = CARTESIAN_POINT ( 'NONE',  ( 3.061616997868383018E-17, 0.000000000000000000, -0.2500000000000000000 ) ) ;
#2963 = ADVANCED_FACE ( 'NONE', ( #12142 ), #10781, .T. ) ;
#2964 = FACE_OUTER_BOUND ( 'NONE', #20175, .T. ) ;
#2965 = CARTESIAN_POINT ( 'NONE',  ( 0.2201042859353726511, 4.078604825199830586, 0.2219247941868362495 ) ) ;
#2966 = CARTESIAN_POINT ( 'NONE',  ( -0.3613381517857143232, 0.3866071427596004528, -4.425116109941954795E-17 ) ) ;
#2967 = CARTESIAN_POINT ( 'NONE',  ( -0.2781420133907471781, 5.053541304894200614, -0.1415874665319149239 ) ) ;
#2968 = EDGE_CURVE ( 'NONE', #20369, #23426, #6909, .T. ) ;
#2969 = VECTOR ( 'NONE', #1708, 39.37007874015748143 ) ;
#2970 = DIRECTION ( 'NONE',  ( -0.000000000000000000, -1.000000000000000000, -0.000000000000000000 ) ) ;
#2971 = FACE_OUTER_BOUND ( 'NONE', #4503, .T. ) ;
#2972 = ORIENTED_EDGE ( 'NONE', *, *, #1279, .F. ) ;
#2973 = CARTESIAN_POINT ( 'NONE',  ( 0.2819296736111110979, 3.766055555631420582, 0.1167790944451422425 ) ) ;
#2974 = CARTESIAN_POINT ( 'NONE',  ( -0.07848227395379105131, 0.04462176029470379945, -0.2841493449351579215 ) ) ;
#2975 = CARTESIAN_POINT ( 'NONE',  ( -4.760580627680044823E-09, 4.932722222506802368, -0.3119999999999999996 ) ) ;
#2976 = CARTESIAN_POINT ( 'NONE',  ( 0.01377311677012589726, 0.04044221366775575116, 0.2899422136677570205 ) ) ;
#2977 = APPLICATION_CONTEXT ( 'configuration controlled 3d designs of mechanical parts and assemblies' ) ;
#2978 = AXIS2_PLACEMENT_3D ( 'NONE', #6692, #10371, #20201 ) ;
#2979 = DIRECTION ( 'NONE',  ( -0.000000000000000000, -1.000000000000000000, -0.000000000000000000 ) ) ;
#2980 = CARTESIAN_POINT ( 'NONE',  ( 0.1292346314604056190, 4.484805555707287006, -0.3119999999999999996 ) ) ;
#2981 = CARTESIAN_POINT ( 'NONE',  ( -0.2819296736111110424, 4.759111111186977716, 0.1167790944451424923 ) ) ;
#2982 = ORIENTED_EDGE ( 'NONE', *, *, #17351, .T. ) ;
#2983 = CARTESIAN_POINT ( 'NONE',  ( -0.1993543840281266355, 4.137583333409199149, 0.1993543840281267465 ) ) ;
#2984 = ORIENTED_EDGE ( 'NONE', *, *, #14455, .T. ) ;
#2985 = ORIENTED_EDGE ( 'NONE', *, *, #13200, .F. ) ;
#2986 = ORIENTED_EDGE ( 'NONE', *, *, #17379, .T. ) ;
#2987 = PERSON_AND_ORGANIZATION ( #15518, #2538 ) ;
#2988 = ORIENTED_EDGE ( 'NONE', *, *, #12774, .F. ) ;
#2989 = PRODUCT_DEFINITION ( 'UNKNOWN', '', #4115, #11942 ) ;
#2990 = CARTESIAN_POINT ( 'NONE',  ( 0.4645897358368414887, 0.2720347660510105681, 0.05893128447555067567 ) ) ;
#2991 = CARTESIAN_POINT ( 'NONE',  ( 1.123474536090420584, 2.661358883302036293, -1.021083823334169027 ) ) ;
#2992 = EDGE_LOOP ( 'NONE', ( #18075, #2910, #10313, #3605 ) ) ;
#2993 = CARTESIAN_POINT ( 'NONE',  ( -0.3119999999999999996, 0.09097222207048931419, -0.1292346314604056745 ) ) ;
#2994 = VECTOR ( 'NONE', #4397, 39.37007874015748143 ) ;
#2995 = CARTESIAN_POINT ( 'NONE',  ( -0.003434916545333202738, 4.377259052997221289, -0.3119838150564986368 ) ) ;
#2996 = CARTESIAN_POINT ( 'NONE',  ( -0.4687500000000003886, -0.2598076211353318454, 0.3779506566538943235 ) ) ;
#2997 = LINE ( 'NONE', #10447, #8911 ) ;
#2998 = ORIENTED_EDGE ( 'NONE', *, *, #843, .F. ) ;
#2999 = ORIENTED_EDGE ( 'NONE', *, *, #1089, .T. ) ;
#3000 = CARTESIAN_POINT ( 'NONE',  ( -0.2764156081756484196, 1.692557448933383907E-17, 0.3661111111111152172 ) ) ;
#3001 = DIRECTION ( 'NONE',  ( -0.000000000000000000, -1.000000000000000000, -0.000000000000000000 ) ) ;
#3002 = CARTESIAN_POINT ( 'NONE',  ( 0.000000000000000000, 0.2764156081756484196, 0.01888888888889020401 ) ) ;
#3003 = CARTESIAN_POINT ( 'NONE',  ( -1.726321361862525858E-17, 4.505638888964754507, -0.2819296736111110979 ) ) ;
#3004 = FACE_OUTER_BOUND ( 'NONE', #15519, .T. ) ;
#3005 = CARTESIAN_POINT ( 'NONE',  ( -0.2081395996546885896, 0.2505969284152432808, -1.206356489598498394 ) ) ;
#3006 = CARTESIAN_POINT ( 'NONE',  ( 1.078523662826197160, 4.111524471938507119, -0.8231847808846625147 ) ) ;
#3007 = CARTESIAN_POINT ( 'NONE',  ( 0.1292346314604058410, 3.957027777777776478, 0.3119999999999998885 ) ) ;
#3008 = CARTESIAN_POINT ( 'NONE',  ( -0.2206173157302028232, 5.106333333485065573, -0.2206173157302028232 ) ) ;
#3009 = CARTESIAN_POINT ( 'NONE',  ( -0.3119999999999998885, 4.665361111111110404, 0.1292346314604058410 ) ) ;
#3010 = EDGE_CURVE ( 'NONE', #3821, #21597, #19550, .T. ) ;
#3011 = ORIENTED_EDGE ( 'NONE', *, *, #19414, .T. ) ;
#3012 = VECTOR ( 'NONE', #713, 39.37007874015748143 ) ;
#3013 = CARTESIAN_POINT ( 'NONE',  ( 0.3155047199421904813, 2.819495280057808362, -0.1294952800578086372 ) ) ;
#3014 = ORIENTED_EDGE ( 'NONE', *, *, #20910, .F. ) ;
#3015 = CARTESIAN_POINT ( 'NONE',  ( -0.2209708691207961095, 0.2209708691207961373, 0.2272222222222253785 ) ) ;
#3016 = EDGE_CURVE ( 'NONE', #20507, #16517, #23434, .T. ) ;
#3017 = CARTESIAN_POINT ( 'NONE',  ( 0.1306872919485616846, 0.3155070326520292290, -0.007152777777776447334 ) ) ;
#3018 = CARTESIAN_POINT ( 'NONE',  ( -6.979263641208234666E-17, 0.4223214284738860402, 0.3799334167787516425 ) ) ;
#3019 = CARTESIAN_POINT ( 'NONE',  ( -0.2206173157302027676, 4.446611111111110404, 0.2206173157302028787 ) ) ;
#3020 = CARTESIAN_POINT ( 'NONE',  ( 0.3613381517857143232, 0.2080357141881718774, 0.000000000000000000 ) ) ;
#3021 = AXIS2_PLACEMENT_3D ( 'NONE', #4971, #21447, #2788 ) ;
#3022 = CARTESIAN_POINT ( 'NONE',  ( 0.1167790944451423535, 0.03888888881302225708, 0.2819296736111110979 ) ) ;
#3023 = CARTESIAN_POINT ( 'NONE',  ( 0.1954553509668047195, 0.1954553509668046085, -0.03666666666666580643 ) ) ;
#3024 = CARTESIAN_POINT ( 'NONE',  ( 0.4805263112511645174, -0.2592867110628498395, 0.04342012612512791137 ) ) ;
#3025 = CARTESIAN_POINT ( 'NONE',  ( -0.1993543840281266910, 5.193138888964755395, -0.1993543840281266910 ) ) ;
#3026 = CARTESIAN_POINT ( 'NONE',  ( -0.2764156081756484196, -0.1144950937579609362, 0.4320833333333378157 ) ) ;
#3027 = ORIENTED_EDGE ( 'NONE', *, *, #23214, .F. ) ;
#3028 = CARTESIAN_POINT ( 'NONE',  ( 0.3119999999999999996, 3.859805555555554601, -0.1292346314604056745 ) ) ;
#3029 = CARTESIAN_POINT ( 'NONE',  ( -8.048972922423762964E-05, 4.293831062076359117, 0.3119999997849208784 ) ) ;
#3030 = DIRECTION ( 'NONE',  ( 6.827562483166858637E-16, 0.9767851838303066581, -0.2142211582677916726 ) ) ;
#3031 = CARTESIAN_POINT ( 'NONE',  ( 0.2206173157302028232, 0.5249999999999996891, -0.2206173157302028232 ) ) ;
#3032 = CARTESIAN_POINT ( 'NONE',  ( -0.1292346314604057023, 4.672305555555554157, 0.3119999999999998885 ) ) ;
#3033 = CARTESIAN_POINT ( 'NONE',  ( 0.1167790944451424506, 4.314666666742532186, 0.2819296736111110424 ) ) ;
#3034 = CARTESIAN_POINT ( 'NONE',  ( 0.1167790944451422702, 3.904944444520310753, -0.2819296736111110424 ) ) ;
#3035 = CARTESIAN_POINT ( 'NONE',  ( 3.820898013339742174E-17, 5.384999999999999787, 0.3119999999999999996 ) ) ;
#3036 = CARTESIAN_POINT ( 'NONE',  ( -0.4622078388679876082, 0.2744100571732864813, 0.3892820121258430133 ) ) ;
#3037 = VERTEX_POINT ( 'NONE', #17851 ) ;
#3038 = CARTESIAN_POINT ( 'NONE',  ( -0.3038794704804686497, 3.999912589447470079, -0.08166535634033041113 ) ) ;
#3039 = CARTESIAN_POINT ( 'NONE',  ( 0.1993543840281266633, 4.609805555631420582, -0.1993543840281266910 ) ) ;
#3040 = DIRECTION ( 'NONE',  ( -0.8660254037844434816, -1.483353696775904202E-31, 0.4999999999999913403 ) ) ;
#3041 = AXIS2_PLACEMENT_3D ( 'NONE', #529, #771, #15652 ) ;
#3042 = EDGE_CURVE ( 'NONE', #4696, #23447, #10424, .T. ) ;
#3043 = APPLICATION_PROTOCOL_DEFINITION ( 'international standard', 'config_control_design', 1994, #12648 ) ;
#3044 = CARTESIAN_POINT ( 'NONE',  ( 1.522235971340160240E-16, 0.1799999999999999933, 1.243000000000000105 ) ) ;
#3045 = CARTESIAN_POINT ( 'NONE',  ( 0.000000000000000000, 0.2764156081756484196, -0.09222222222222178911 ) ) ;
#3046 = CARTESIAN_POINT ( 'NONE',  ( -0.1993543840281266355, 4.040361111186976828, 0.1993543840281267465 ) ) ;
#3047 = CARTESIAN_POINT ( 'NONE',  ( -0.3120000000000000551, 0.3826388888888884732, 0.1292346314604056190 ) ) ;
#3048 = CARTESIAN_POINT ( 'NONE',  ( 0.000000000000000000, 5.384999999999999787, 0.000000000000000000 ) ) ;
#3049 = CARTESIAN_POINT ( 'NONE',  ( -0.1144950937579609779, 0.2764156081756484196, 0.1404166666666689378 ) ) ;
#3050 = CARTESIAN_POINT ( 'NONE',  ( -0.2233192592356399442, 0.03660714275960044034, -0.3073725909049500049 ) ) ;
#3051 = CARTESIAN_POINT ( 'NONE',  ( -0.2819296736111110979, 0.5805555554796888451, 0.1167790944451422425 ) ) ;
#3052 = CARTESIAN_POINT ( 'NONE',  ( -0.2245903949464531368, 0.1902879574984994715, 0.4054134354953847219 ) ) ;
#3053 = CARTESIAN_POINT ( 'NONE',  ( 3.799666666666678072, 1.876333333333333631, -1.727333333333314291 ) ) ;
#3054 = CARTESIAN_POINT ( 'NONE',  ( 5.731347020009612645E-17, 4.231333333333332725, 0.3119999999999999996 ) ) ;
#3055 = CARTESIAN_POINT ( 'NONE',  ( 0.1144950937579609085, -0.2764156081756484751, 0.1056944444444464365 ) ) ;
#3056 = CARTESIAN_POINT ( 'NONE',  ( -0.1306872919485615459, -0.3155070326520293400, 0.4060416666666709640 ) ) ;
#3057 = EDGE_LOOP ( 'NONE', ( #20706, #20013, #22616, #10692 ) ) ;
#3058 = ORIENTED_EDGE ( 'NONE', *, *, #6477, .T. ) ;
#3059 = CARTESIAN_POINT ( 'NONE',  ( 0.4449999999999992295, 0.04999999999999919092, 0.000000000000000000 ) ) ;
#3060 = CARTESIAN_POINT ( 'NONE',  ( 0.4687499999998496758, 0.2209570500825255579, 0.4011790492569353161 ) ) ;
#3061 = CARTESIAN_POINT ( 'NONE',  ( -0.2819296736111110424, 0.3374999999241334314, -0.1167790944451423396 ) ) ;
#3062 = CARTESIAN_POINT ( 'NONE',  ( 5.178964085587577574E-17, 4.158416666742532186, 0.2819296736111110979 ) ) ;
#3063 = VECTOR ( 'NONE', #7733, 39.37007874015748143 ) ;
#3064 = CARTESIAN_POINT ( 'NONE',  ( 0.2233192592356399164, 0.0008928570453147541665, 0.3073725909049500604 ) ) ;
#3065 = VERTEX_POINT ( 'NONE', #12616 ) ;
#3066 = CARTESIAN_POINT ( 'NONE',  ( 0.1167790944451424368, 4.717444444520309865, 0.2819296736111110424 ) ) ;
#3067 = CARTESIAN_POINT ( 'NONE',  ( 0.2660021697418833431, 5.126719186317235000, 0.1552671348293162834 ) ) ;
#3068 = EDGE_CURVE ( 'NONE', #4326, #19937, #6505, .T. ) ;
#3069 = CARTESIAN_POINT ( 'NONE',  ( 0.2382335091060892029, 5.084669797853266893, -0.2016295426171259009 ) ) ;
#3070 = EDGE_CURVE ( 'NONE', #9832, #15369, #6743, .T. ) ;
#3071 = FACE_OUTER_BOUND ( 'NONE', #17815, .T. ) ;
#3072 = CARTESIAN_POINT ( 'NONE',  ( -0.2819296736111110424, 5.071611111186976828, -0.1167790944451423119 ) ) ;
#3073 = CARTESIAN_POINT ( 'NONE',  ( 0.2645723224789517936, 4.191640340208213189, 0.1653647831739661345 ) ) ;
#3074 = ADVANCED_FACE ( 'NONE', ( #14187 ), #21384, .T. ) ;
#3075 =( BOUNDED_CURVE ( )  B_SPLINE_CURVE ( 2, ( #14722, #7510, #22137, #16542, #16660, #5556, #16777, #5437, #3852, #12903, #22376, #13142, #23963, #13259, #14596, #7626, #5794, #18724, #10818, #18606, #20555, #3603, #11054, #7390, #22260, #13020, #20435, #3732, #1899, #9461, #16893, #20674, #18246, #1543, #8975, #3486, #23833, #22018, #5315, #12778, #20198, #10936, #18364, #1658, #2623, #11905, #23084, #4204, #21028, #9701, #2143, #15311, #17140, #11658, #427, #19081, #22627, #8215, #15189, #8094, #11538, #7979, #15548, #2388, #9580, #20911, #13844, #22739, #665, #543, #19325, #9825, #2266, #6027, #18969, #5912, #22969, #11775, #3967, #11412, #13496, #10066, #17260, #19196, #15430, #17491, #13370, #786, #18845, #15664, #17375, #17012, #7746, #22857, #6147, #2505, #13613, #6392, #9945, #305, #20790, #7861, #4320, #4081, #6270, #13728, #21151, #4438, #8335, #10308, #14199, #21632, #1027, #8589, #8457, #23683, #1151, #12263, #15900, #23565, #10662, #6880, #19678, #21754, #16150, #18093, #6630, #19804, #6515, #2981, #19438, #14078, #2738, #1272, #21507, #4924, #7004, #4799, #16026, #14321, #21393, #10435, #23442, #3101, #23322, #5040, #17859, #8699, #10548, #19559, #21274, #904, #1394, #16271, #12507, #4565, #12388, #17981, #4682, #6754, #19929, #3215, #8825, #12024, #2850, #10190, #17613, #15786, #23204, #13963, #12152, #17732, #16396, #5285, #3457, #18578, #9192, #12873, #7480, #23804, #14927, #1868, #3700, #22347, #9066, #11028, #21990, #12629, #20169, #12753, #1632, #10908, #16514, #18219, #32, #10791, #14813, #7125, #14567, #22230, #14447, #20045, #23928, #21871, #7247, #1749, #18337, #3334, #14693, #22111, #5406, #20290, #3575, #8948, #5163, #18455, #9308, #16634, #24052, #16750, #1513, #5529, #7362, #12993, #20408, #11147, #15378, #4391, #17323, #11978, #5976, #17564, #20738, #19390, #10020, #2218, #374, #8048, #2455, #19267, #6221, #13568, #22925, #23150, #15256, #11605, #13685, #618, #22807, #11481, #15737, #4031, #8285, #7924, #22686, #2571, #11726, #6098, #4153, #21101, #11851, #19148, #20976, #23037, #10141, #6461, #17083, #2688, #21222, #9893, #737, #17208, #17443, #4273, #9648, #15498, #8166, #15620, #6341, #855, #18916, #13793, #4512, #7815, #20859, #492, #13440, #19035, #9773, #2337, #1095, #14143, #10381, #1458, #1335, #14264, #4984, #4744, #12215, #8402, #15970, #10610, #14030, #23391, #19868, #8765, #6698, #19749, #3160, #1218, #19624, #21572, #14386, #18039, #12449, #21701, #5103, #8646, #19989, #10493, #4866, #16094, #8893, #6580, #16336, #12569, #6948, #3277, #23747, #10255, #10730, #21814, #12333, #16218, #17803, #23630, #3046, #19507, #17923, #23508, #18161, #6823, #13914, #21342, #4629, #12097, #2800, #21460, #8526, #973, #17682, #2921, #15852, #23269, #7639, #3863, #19092, #18979, #7757, #22637, #22388, #7871, #7071, #15201, #4092, #7517, #16904, #13381, #2277, #198, #13269, #20804, #18858, #5689, #15088, #15320, #11549, #5922, #9713, #22751, #2159, #18736, #6042, #17150, #9592, #2399, #74, #9838, #13508, #440, #22510, #21928, #4215, #1579, #2033, #17270, #20922, #10853, #17024, #11668, #13152, #318, #14509, #11426, #5221, #12694, #20111, #5804, #3403, #20685, #18281, #16792, #9014, #3976, #14966, #20565, #11305, #9470, #15556, #11784, #12160, #13972, #6159, #4333, #12037 ),
 .UNSPECIFIED., .F., .T. ) 
 B_SPLINE_CURVE_WITH_KNOTS ( ( 3, 2, 2, 2, 2, 2, 2, 2, 2, 2, 2, 2, 2, 2, 2, 2, 2, 2, 2, 2, 2, 2, 2, 2, 2, 2, 2, 2, 2, 2, 2, 2, 2, 2, 2, 2, 2, 2, 2, 2, 2, 2, 2, 2, 2, 2, 2, 2, 2, 2, 2, 2, 2, 2, 2, 2, 2, 2, 2, 2, 2, 2, 2, 2, 2, 2, 2, 2, 2, 2, 2, 2, 2, 2, 2, 2, 2, 2, 2, 2, 2, 2, 2, 2, 2, 2, 2, 2, 2, 2, 2, 2, 2, 2, 2, 2, 2, 2, 2, 2, 2, 2, 2, 2, 2, 2, 2, 2, 2, 2, 2, 2, 2, 2, 2, 2, 2, 2, 2, 2, 2, 2, 2, 2, 2, 2, 2, 2, 2, 2, 2, 2, 2, 2, 2, 2, 2, 2, 2, 2, 2, 2, 2, 2, 2, 2, 2, 2, 2, 2, 2, 2, 2, 2, 2, 2, 2, 2, 2, 2, 2, 2, 2, 2, 2, 2, 2, 2, 2, 2, 2, 2, 2, 2, 2, 2, 2, 2, 2, 2, 2, 2, 2, 2, 2, 2, 2, 2, 2, 2, 2, 2, 2, 2, 2, 2, 2, 2, 2, 2, 2, 2, 2, 2, 2, 2, 2, 2, 2, 2, 2, 2, 3 ),
 ( 0.03225371760371920082, 0.03655005604694450128, 0.04111881305281361171, 0.04568757005868272214, 0.05025632706455182563, 0.05482508407042094301, 0.05939384107629005344, 0.06396259808215916387, 0.06853135508802826736, 0.07310011209389738474, 0.07766886909976648823, 0.08223762610563560560, 0.08680638311150470909, 0.09137514011737382646, 0.09594389712324292996, 0.1005126541291120335, 0.1050814111349811369, 0.1096501681408502543, 0.1142189251467193856, 0.1187876821525884752, 0.1233564391584576064, 0.1279251961643266822, 0.1324939531701957995, 0.1370627101760649169, 0.1416314671819340343, 0.1462002241878031239, 0.1507689811936722690, 0.1553377381995413309, 0.1599064952054104760, 0.1644752522112795934, 0.1690440092171486830, 0.1736127662230178004, 0.1781815232288868900, 0.1827502802347560074, 0.1873190372406251247, 0.1918877942464942421, 0.1964565512523633317, 0.2010253082582324491, 0.2055940652641015665, 0.2101628222699706838, 0.2147315792758397734, 0.2193003362817088908, 0.2238690932875780082, 0.2284378502934471256, 0.2330066072993162152, 0.2375753643051853325, 0.2421441213110544499, 0.2467128783169235673, 0.2512816353227926292, 0.2558503923286618020, 0.2604191493345308639, 0.2649879063404000368, 0.2695566633462690986, 0.2741254203521382160, 0.2786941773580072779, 0.2832629343638764507, 0.2878316913697455126, 0.2924004483756146300, 0.2969692053814838029, 0.3015379623873529202, 0.3061067193932219821, 0.3106754763990910995, 0.3152442334049602168, 0.3198129904108292787, 0.3243817474166983961, 0.3289505044225675690, 0.3335192614284366308, 0.3380880184343057482, 0.3426567754401748656, 0.3472255324460440384, 0.3517942894519130448, 0.3563630464577821622, 0.3609318034636513350, 0.3655005604695203969, 0.3700693174753895143, 0.3746380744812586316, 0.3792068314871278045, 0.3837755884929968664, 0.3883443454988659282, 0.3929131025047351011, 0.3974818595106041630, 0.4020506165164732804, 0.4066193735223423977, 0.4111881305282115706, 0.4157568875340806325, 0.4203256445399497498, 0.4248944015458188672, 0.4294631585516879291, 0.4340319155575570464, 0.4386006725634261638, 0.4431694295692952812, 0.4477381865751643986, 0.4523069435810335159, 0.4568757005869026888, 0.4614444575927716952, 0.4660132145986408125, 0.4705819716045099299, 0.4751507286103790473, 0.4797194856162481646, 0.4842882426221172820, 0.4888569996279864549, 0.4934257566338555168, 0.4979945136397245786, 0.5025632706455936960, 0.5071320276514628134, 0.5117007846573319307, 0.5162695416632010481, 0.5208382986690700545, 0.5254070556749392829, 0.5299758126808085112, 0.5345445696866775176, 0.5391133266925466350, 0.5436820836984157523, 0.5482508407042848697, 0.5528195977101539871, 0.5573883547160231045, 0.5619571117218922218, 0.5665258687277613392, 0.5710946257336304566, 0.5756633827394995739, 0.5802321397453686913, 0.5848008967512376977, 0.5893696537571068150, 0.5939384107629760434, 0.5985071677688450498, 0.6030759247747142782, 0.6076446817805832845, 0.6122134387864524019, 0.6167821957923215193, 0.6213509527981906366, 0.6259197098040597540, 0.6304884668099288714, 0.6350572238157979887, 0.6396259808216669951, 0.6441947378275362235, 0.6487634948334052298, 0.6533322518392744582, 0.6579010088451435756, 0.6624697658510125819, 0.6670385228568818103, 0.6716072798627508167, 0.6761760368686199341, 0.6807447938744890514, 0.6853135508803581688, 0.6898823078862272862, 0.6944510648920965146, 0.6990198218979655209, 0.7035885789038345273, 0.7081573359097037557, 0.7127260929155727620, 0.7172948499214418794, 0.7218636069273111078, 0.7264323639331802251, 0.7310011209390493425, 0.7355698779449183489, 0.7401386349507874662, 0.7447073919566565836, 0.7492761489625257010, 0.7538449059683948184, 0.7584136629742640467, 0.7629824199801330531, 0.7675511769860021705, 0.7721199339918712878, 0.7766886909977402942, 0.7812574480036094116, 0.7858262050094786400, 0.7903949620153477573, 0.7949637190212168747, 0.7995324760270859921, 0.8041012330329549984, 0.8086699900388241158, 0.8132387470446932332, 0.8178075040505623505, 0.8223762610564315789, 0.8269450180623005853, 0.8315137750681697026, 0.8360825320740388200, 0.8406512890799079374, 0.8452200460857769437, 0.8497888030916461721, 0.8543575600975152895, 0.8589263171033842958, 0.8634950741092535242, 0.8680638311151225306, 0.8726325881209917590, 0.8772013451268607653, 0.8817701021327298827, 0.8863388591385991111, 0.8909076161444681174, 0.8954763731503372348, 0.9000451301562063522, 0.9046138871620754696, 0.9091826441679444759, 0.9137514011738138153, 0.9183201581796828217, 0.9228889151855518280, 0.9274576721914210564, 0.9320264291972900628, 0.9365951862031591801, 0.9411639432090282975, 0.9457327002148975259, 0.9503014572207666433, 0.9548702142266356496, 0.9594389712325047670, 0.9640077282383738844, 0.9685764852442430017, 0.9731452422501120081, 0.9777139992559813475, 0.9822827562618503539, 0.9868515132677194712, 0.9914202702735885886, 0.9959890272794575949, 1.000000000000000000 ),
 .UNSPECIFIED. ) 
 CURVE ( )  GEOMETRIC_REPRESENTATION_ITEM ( )  RATIONAL_B_SPLINE_CURVE ( ( 0.9914636835865273667, 0.9284183224522731814, 1.000000000000000000, 0.9238795325112867385, 1.000000000000000000, 0.9238795325112867385, 1.000000000000000000, 0.9238795325112867385, 1.000000000000000000, 0.9238795325112867385, 1.000000000000000000, 0.9238795325112867385, 1.000000000000000000, 0.9238795325112867385, 1.000000000000000000, 0.9238795325112867385, 1.000000000000000000, 0.9238795325112867385, 1.000000000000000000, 0.9238795325112867385, 1.000000000000000000, 0.9238795325112867385, 1.000000000000000000, 0.9238795325112867385, 1.000000000000000000, 0.9238795325112867385, 1.000000000000000000, 0.9238795325112867385, 1.000000000000000000, 0.9238795325112867385, 1.000000000000000000, 0.9238795325112867385, 1.000000000000000000, 0.9238795325112867385, 1.000000000000000000, 0.9238795325112867385, 1.000000000000000000, 0.9238795325112867385, 1.000000000000000000, 0.9238795325112867385, 1.000000000000000000, 0.9238795325112867385, 1.000000000000000000, 0.9238795325112867385, 1.000000000000000000, 0.9238795325112867385, 1.000000000000000000, 0.9238795325112867385, 1.000000000000000000, 0.9238795325112867385, 1.000000000000000000, 0.9238795325112867385, 1.000000000000000000, 0.9238795325112867385, 1.000000000000000000, 0.9238795325112867385, 1.000000000000000000, 0.9238795325112867385, 1.000000000000000000, 0.9238795325112867385, 1.000000000000000000, 0.9238795325112867385, 1.000000000000000000, 0.9238795325112867385, 1.000000000000000000, 0.9238795325112867385, 1.000000000000000000, 0.9238795325112867385, 1.000000000000000000, 0.9238795325112867385, 1.000000000000000000, 0.9238795325112867385, 1.000000000000000000, 0.9238795325112867385, 1.000000000000000000, 0.9238795325112867385, 1.000000000000000000, 0.9238795325112867385, 1.000000000000000000, 0.9238795325112867385, 1.000000000000000000, 0.9238795325112867385, 1.000000000000000000, 0.9238795325112867385, 1.000000000000000000, 0.9238795325112867385, 1.000000000000000000, 0.9238795325112867385, 1.000000000000000000, 0.9238795325112867385, 1.000000000000000000, 0.9238795325112867385, 1.000000000000000000, 0.9238795325112867385, 1.000000000000000000, 0.9238795325112867385, 1.000000000000000000, 0.9238795325112867385, 1.000000000000000000, 0.9238795325112867385, 1.000000000000000000, 0.9238795325112867385, 1.000000000000000000, 0.9238795325112867385, 1.000000000000000000, 0.9238795325112867385, 1.000000000000000000, 0.9238795325112867385, 1.000000000000000000, 0.9238795325112867385, 1.000000000000000000, 0.9238795325112867385, 1.000000000000000000, 0.9238795325112867385, 1.000000000000000000, 0.9238795325112867385, 1.000000000000000000, 0.9238795325112867385, 1.000000000000000000, 0.9238795325112867385, 1.000000000000000000, 0.9238795325112867385, 1.000000000000000000, 0.9238795325112867385, 1.000000000000000000, 0.9238795325112867385, 1.000000000000000000, 0.9238795325112867385, 1.000000000000000000, 0.9238795325112867385, 1.000000000000000000, 0.9238795325112867385, 1.000000000000000000, 0.9238795325112867385, 1.000000000000000000, 0.9238795325112867385, 1.000000000000000000, 0.9238795325112867385, 1.000000000000000000, 0.9238795325112867385, 1.000000000000000000, 0.9238795325112867385, 1.000000000000000000, 0.9238795325112867385, 1.000000000000000000, 0.9238795325112867385, 1.000000000000000000, 0.9238795325112867385, 1.000000000000000000, 0.9238795325112867385, 1.000000000000000000, 0.9238795325112867385, 1.000000000000000000, 0.9238795325112867385, 1.000000000000000000, 0.9238795325112867385, 1.000000000000000000, 0.9238795325112867385, 1.000000000000000000, 0.9238795325112867385, 1.000000000000000000, 0.9238795325112867385, 1.000000000000000000, 0.9238795325112867385, 1.000000000000000000, 0.9238795325112867385, 1.000000000000000000, 0.9238795325112867385, 1.000000000000000000, 0.9238795325112867385, 1.000000000000000000, 0.9238795325112867385, 1.000000000000000000, 0.9238795325112867385, 1.000000000000000000, 0.9238795325112867385, 1.000000000000000000, 0.9238795325112867385, 1.000000000000000000, 0.9238795325112867385, 1.000000000000000000, 0.9238795325112867385, 1.000000000000000000, 0.9238795325112867385, 1.000000000000000000, 0.9238795325112867385, 1.000000000000000000, 0.9238795325112867385, 1.000000000000000000, 0.9238795325112867385, 1.000000000000000000, 0.9238795325112867385, 1.000000000000000000, 0.9238795325112867385, 1.000000000000000000, 0.9238795325112867385, 1.000000000000000000, 0.9238795325112867385, 1.000000000000000000, 0.9238795325112867385, 1.000000000000000000, 0.9238795325112867385, 1.000000000000000000, 0.9238795325112867385, 1.000000000000000000, 0.9238795325112867385, 1.000000000000000000, 0.9238795325112867385, 1.000000000000000000, 0.9238795325112867385, 1.000000000000000000, 0.9238795325112867385, 1.000000000000000000, 0.9238795325112867385, 1.000000000000000000, 0.9238795325112867385, 1.000000000000000000, 0.9238795325112867385, 1.000000000000000000, 0.9238795325112867385, 1.000000000000000000, 0.9238795325112867385, 1.000000000000000000, 0.9238795325112867385, 1.000000000000000000, 0.9238795325112867385, 1.000000000000000000, 0.9238795325112867385, 1.000000000000000000, 0.9238795325112867385, 1.000000000000000000, 0.9238795325112867385, 1.000000000000000000, 0.9238795325112867385, 1.000000000000000000, 0.9238795325112867385, 1.000000000000000000, 0.9238795325112867385, 1.000000000000000000, 0.9238795325112867385, 1.000000000000000000, 0.9238795325112867385, 1.000000000000000000, 0.9238795325112867385, 1.000000000000000000, 0.9238795325112867385, 1.000000000000000000, 0.9238795325112867385, 1.000000000000000000, 0.9238795325112867385, 1.000000000000000000, 0.9238795325112867385, 1.000000000000000000, 0.9238795325112867385, 1.000000000000000000, 0.9238795325112867385, 1.000000000000000000, 0.9238795325112867385, 1.000000000000000000, 0.9238795325112867385, 1.000000000000000000, 0.9238795325112867385, 1.000000000000000000, 0.9238795325112867385, 1.000000000000000000, 0.9238795325112867385, 1.000000000000000000, 0.9238795325112867385, 1.000000000000000000, 0.9238795325112867385, 1.000000000000000000, 0.9238795325112867385, 1.000000000000000000, 0.9238795325112867385, 1.000000000000000000, 0.9238795325112867385, 1.000000000000000000, 0.9238795325112867385, 1.000000000000000000, 0.9238795325112867385, 1.000000000000000000, 0.9238795325112867385, 1.000000000000000000, 0.9238795325112867385, 1.000000000000000000, 0.9238795325112867385, 1.000000000000000000, 0.9238795325112867385, 1.000000000000000000, 0.9238795325112867385, 1.000000000000000000, 0.9238795325112867385, 1.000000000000000000, 0.9238795325112867385, 1.000000000000000000, 0.9238795325112867385, 1.000000000000000000, 0.9238795325112867385, 1.000000000000000000, 0.9238795325112867385, 1.000000000000000000, 0.9238795325112867385, 1.000000000000000000, 0.9238795325112867385, 1.000000000000000000, 0.9238795325112867385, 1.000000000000000000, 0.9238795325112867385, 1.000000000000000000, 0.9238795325112867385, 1.000000000000000000, 0.9238795325112867385, 1.000000000000000000, 0.9238795325112867385, 1.000000000000000000, 0.9238795325112867385, 1.000000000000000000, 0.9238795325112867385, 1.000000000000000000, 0.9238795325112867385, 1.000000000000000000, 0.9238795325112867385, 1.000000000000000000, 0.9238795325112867385, 1.000000000000000000, 0.9238795325112867385, 1.000000000000000000, 0.9238795325112867385, 1.000000000000000000, 0.9238795325112867385, 1.000000000000000000, 0.9238795325112867385, 1.000000000000000000, 0.9238795325112867385, 1.000000000000000000, 0.9238795325112867385, 1.000000000000000000, 0.9238795325112867385, 1.000000000000000000, 0.9238795325112867385, 1.000000000000000000, 0.9238795325112867385, 1.000000000000000000, 0.9238795325112867385, 1.000000000000000000, 0.9238795325112867385, 1.000000000000000000, 0.9238795325112867385, 1.000000000000000000, 0.9238795325112867385, 1.000000000000000000, 0.9238795325112867385, 1.000000000000000000, 0.9238795325112867385, 1.000000000000000000, 0.9238795325112867385, 1.000000000000000000, 0.9238795325112867385, 1.000000000000000000, 0.9238795325112867385, 1.000000000000000000, 0.9238795325112867385, 1.000000000000000000, 0.9238795325112867385, 1.000000000000000000, 0.9238795325112867385, 1.000000000000000000, 0.9238795325112867385, 1.000000000000000000, 0.9238795325112867385, 1.000000000000000000, 0.9238795325112867385, 1.000000000000000000, 0.9238795325112867385, 1.000000000000000000, 0.9238795325112867385, 1.000000000000000000, 0.9238795325112867385, 1.000000000000000000, 0.9238795325112867385, 1.000000000000000000, 0.9238795325112867385, 1.000000000000000000, 0.9238795325112867385, 1.000000000000000000, 0.9238795325112867385, 1.000000000000000000, 0.9238795325112867385, 1.000000000000000000, 0.9238795325112867385, 1.000000000000000000, 0.9238795325112867385, 1.000000000000000000, 0.9238795325112867385, 1.000000000000000000, 0.9238795325112867385, 1.000000000000000000, 0.9238795325112867385, 1.000000000000000000, 0.9238795325112867385, 1.000000000000000000, 0.9238795325112867385, 1.000000000000000000, 0.9238795325112867385, 1.000000000000000000, 0.9238795325112867385, 1.000000000000000000, 0.9238795325112867385, 1.000000000000000000, 0.9238795325112867385, 1.000000000000000000, 0.9238795325112867385, 1.000000000000000000, 0.9238795325112867385, 1.000000000000000000, 0.9238795325112867385, 1.000000000000000000, 0.9238795325112867385, 1.000000000000000000, 0.9238795325112867385, 1.000000000000000000, 0.9238795325112867385, 1.000000000000000000, 0.9331728261800869006, 0.9836825870399050764 ) ) 
 REPRESENTATION_ITEM ( '' )  );
#3076 = CARTESIAN_POINT ( 'NONE',  ( 0.07168957172816003975, 0.03242967361111057795, 0.2730421076994219431 ) ) ;
#3077 =( BOUNDED_CURVE ( )  B_SPLINE_CURVE ( 2, ( #23861, #8755, #7422, #12562, #5344, #5583, #20345, #14376, #12808 ),
 .UNSPECIFIED., .F., .T. ) 
 B_SPLINE_CURVE_WITH_KNOTS ( ( 3, 2, 2, 2, 3 ),
 ( 0.8660714285714284921, 0.8705357142857141906, 0.8750000000000000000, 0.8794642857142856984, 0.8839285714285713969 ),
 .UNSPECIFIED. ) 
 CURVE ( )  GEOMETRIC_REPRESENTATION_ITEM ( )  RATIONAL_B_SPLINE_CURVE ( ( 1.000000000000001998, 0.9238795325112848511, 1.000000000000000000, 0.9238795325112867385, 1.000000000000000000, 0.9238795325112867385, 1.000000000000000000, 0.9238795325112867385, 1.000000000000000000 ) ) 
 REPRESENTATION_ITEM ( '' )  );
#3078 = AXIS2_PLACEMENT_3D ( 'NONE', #15453, #11793, #16912 ) ;
#3079 = CARTESIAN_POINT ( 'NONE',  ( 0.1167790944451424506, 4.925777777853642903, 0.2819296736111110424 ) ) ;
#3080 = DATE_AND_TIME ( #6610, #2570 ) ;
#3081 = ORIENTED_EDGE ( 'NONE', *, *, #17650, .F. ) ;
#3082 = CARTESIAN_POINT ( 'NONE',  ( -0.08027973808803456901, 5.102470732942563814, -0.3007383443984451565 ) ) ;
#3083 = CARTESIAN_POINT ( 'NONE',  ( -0.3119999999999999996, 0.2055555554038226151, -3.820898013339742174E-17 ) ) ;
#3085 = ORIENTED_EDGE ( 'NONE', *, *, #3366, .T. ) ;
#3084 = B_SPLINE_CURVE_WITH_KNOTS ( 'NONE', 3,
 ( #23763, #19521, #8908, #16233, #988, #6595, #6838, #1234, #14403, #4999, #14523, #5117, #21946, #5238, #4882, #2815, #8417, #8659 ),
 .UNSPECIFIED., .F., .F.,
 ( 4, 2, 2, 2, 2, 2, 2, 2, 4 ),
 ( 0.9046139031640043626, 0.9068982821206797995, 0.9091826610773552364, 0.9114670400340306733, 0.9137514189907061102, 0.9160357979473815471, 0.9183201769040569840, 0.9206045558607324208, 0.9228889348174078577 ),
 .UNSPECIFIED. ) ;
#3086 = CARTESIAN_POINT ( 'NONE',  ( -0.2819296736111110979, 0.1916666665908000333, 0.1167790944451422425 ) ) ;
#3087 = CARTESIAN_POINT ( 'NONE',  ( 0.2819296736111110979, 0.04930555547968892144, 0.000000000000000000 ) ) ;
#3088 = CARTESIAN_POINT ( 'NONE',  ( 0.000000000000000000, 5.384999999999999787, 0.000000000000000000 ) ) ;
#3089 = CARTESIAN_POINT ( 'NONE',  ( 7.515426412127797749E-07, 4.849418923572540230, 0.3119999999980542227 ) ) ;
#3090 = CARTESIAN_POINT ( 'NONE',  ( 0.1236067977499789861, -0.01428571428571431129, -0.3804226065180614236 ) ) ;
#3091 = CARTESIAN_POINT ( 'NONE',  ( -0.2882663752280904546, 5.054250704846746878, -0.1193744778696609748 ) ) ;
#3092 = DIRECTION ( 'NONE',  ( -1.000000000000000000, 0.000000000000000000, 0.000000000000000000 ) ) ;
#3093 = DIRECTION ( 'NONE',  ( 0.8660254037844435926, 0.000000000000000000, 0.4999999999999914513 ) ) ;
#3094 = CARTESIAN_POINT ( 'NONE',  ( -0.1167790944451423535, 4.821611111186976828, 0.2819296736111110424 ) ) ;
#3095 = DIRECTION ( 'NONE',  ( 0.2455557836931403226, -0.6854569122471694254, 0.6854569122471694254 ) ) ;
#3096 = CARTESIAN_POINT ( 'NONE',  ( -0.2819296736111110424, 3.800777777853643347, 0.1167790944451424923 ) ) ;
#3097 = CARTESIAN_POINT ( 'NONE',  ( -0.3120000000000000551, 0.09791666651493373397, 0.1292346314604056190 ) ) ;
#3098 = CARTESIAN_POINT ( 'NONE',  ( -0.4645897358368417107, -0.2720347660510102905, 0.05893128447555207733 ) ) ;
#3099 = CARTESIAN_POINT ( 'NONE',  ( -0.3999999999999999667, 0.2089285712334865985, -0.1299678784931626030 ) ) ;
#3100 = CARTESIAN_POINT ( 'NONE',  ( 0.1292346314604056190, 4.318138889040620931, -0.3119999999999999996 ) ) ;
#3101 = CARTESIAN_POINT ( 'NONE',  ( -0.1167790944451423535, 4.710500000075865223, 0.2819296736111110979 ) ) ;
#3102 = ORIENTED_EDGE ( 'NONE', *, *, #17350, .T. ) ;
#3103 = CARTESIAN_POINT ( 'NONE',  ( 0.1167790944451424368, 3.759111111186976828, 0.2819296736111110424 ) ) ;
#3104 = ORIENTED_EDGE ( 'NONE', *, *, #3237, .F. ) ;
#3105 = EDGE_CURVE ( 'NONE', #8144, #8315, #16645, .T. ) ;
#3106 = PRODUCT_DEFINITION_SHAPE ( 'NONE', 'NONE',  #15678 ) ;
#3107 = COORDINATED_UNIVERSAL_TIME_OFFSET ( 0, 0, .AHEAD. ) ;
#3108 = LINE ( 'NONE', #16404, #14629 ) ;
#3109 = CARTESIAN_POINT ( 'NONE',  ( 1.645216030923674522, 2.291712385858714729, -2.498788568296995916 ) ) ;
#3110 = ORIENTED_EDGE ( 'NONE', *, *, #8595, .F. ) ;
#3111 = CARTESIAN_POINT ( 'NONE',  ( -0.3119999999999999996, 0.3756944442927114824, 0.1292346314604056190 ) ) ;
#3112 = CONICAL_SURFACE ( 'NONE', #16747, 0.3125000000000000000, 0.7853981633974497223 ) ;
#3113 = CARTESIAN_POINT ( 'NONE',  ( -0.08648628660923504685, 4.379571832817274135, -0.3004572054626405420 ) ) ;
#3114 = CARTESIAN_POINT ( 'NONE',  ( -0.4687500000000386913, 0.04471557274272623672, 0.4289752932571493926 ) ) ;
#3115 = CARTESIAN_POINT ( 'NONE',  ( 0.2031523753197612414, 0.4269420615838216970, -0.7219681823230330586 ) ) ;
#3116 = ORIENTED_EDGE ( 'NONE', *, *, #670, .T. ) ;
#3117 = DIRECTION ( 'NONE',  ( 0.000000000000000000, 0.000000000000000000, 1.000000000000000000 ) ) ;
#3118 = DIRECTION ( 'NONE',  ( 0.000000000000000000, -1.000000000000000000, 0.000000000000000000 ) ) ;
#3119 = CARTESIAN_POINT ( 'NONE',  ( 0.1954553509668047195, 0.1954553509668046085, 0.1230555555555576941 ) ) ;
#3120 = CARTESIAN_POINT ( 'NONE',  ( 0.2819296736111110424, 4.384111111186976828, -0.1167790944451423396 ) ) ;
#3121 = CARTESIAN_POINT ( 'NONE',  ( -0.1038682246014046850, 0.2678606782618252469, -0.07599903378259419140 ) ) ;
#3122 = CARTESIAN_POINT ( 'NONE',  ( -0.08173883172107287987, 0.7775208687833771171, -1.079850767775349940 ) ) ;
#3123 = DIRECTION ( 'NONE',  ( -1.000000000000000000, 0.000000000000000000, 0.000000000000000000 ) ) ;
#3124 = CARTESIAN_POINT ( 'NONE',  ( -0.04077505786994410630, 4.211656132442665346, -0.3119997438092615427 ) ) ;
#3125 = CARTESIAN_POINT ( 'NONE',  ( 0.3119999999999999996, 4.026472222222221120, -0.1292346314604056745 ) ) ;
#3126 = CARTESIAN_POINT ( 'NONE',  ( 0.1292346314604058410, 5.075083333485064685, 0.3119999999999998885 ) ) ;
#3127 = AXIS2_PLACEMENT_3D ( 'NONE', #838, #17305, #13306 ) ;
#3128 = VECTOR ( 'NONE', #2846, 39.37007874015748143 ) ;
#3129 = CARTESIAN_POINT ( 'NONE',  ( 1.059513921322799533E-10, 3.821611107313654720, -0.3119999999999999996 ) ) ;
#3130 = ORIENTED_EDGE ( 'NONE', *, *, #5798, .T. ) ;
#3131 = PLANE ( 'NONE',  #14599 ) ;
#3132 = CARTESIAN_POINT ( 'NONE',  ( -0.2230971623002953874, 0.2230971623002954152, 0.003263888888890301588 ) ) ;
#3133 = CARTESIAN_POINT ( 'NONE',  ( 2.326421213736078119E-17, 0.3866071427596002308, -0.3799334167787516425 ) ) ;
#3134 = CARTESIAN_POINT ( 'NONE',  ( 4.194415287079685308E-17, -2.347681869555226049E-17, -0.3425000000000000266 ) ) ;
#3135 = VECTOR ( 'NONE', #23066, 39.37007874015748854 ) ;
#3136 = EDGE_CURVE ( 'NONE', #18090, #19497, #8813, .T. ) ;
#3137 = CARTESIAN_POINT ( 'NONE',  ( -0.2923287055106771337, 0.1080357141881718719, 0.2123892367102619971 ) ) ;
#3138 = AXIS2_PLACEMENT_3D ( 'NONE', #19026, #17311, #8036 ) ;
#3139 = CARTESIAN_POINT ( 'NONE',  ( -0.1167790944451424506, 0.1430555554796889284, 0.2819296736111110424 ) ) ;
#3140 = CARTESIAN_POINT ( 'NONE',  ( -0.2764156081756484196, 1.692557448933383907E-17, -0.01583333333333230425 ) ) ;
#3141 = CARTESIAN_POINT ( 'NONE',  ( -0.1954553509668046918, -0.1954553509668046640, 0.4355555555555601921 ) ) ;
#3142 = ORIENTED_EDGE ( 'NONE', *, *, #19990, .F. ) ;
#3143 = CARTESIAN_POINT ( 'NONE',  ( 2.583392422801336671E-17, 0.1199999999999999678, 0.2109499999999995268 ) ) ;
#3144 = CARTESIAN_POINT ( 'NONE',  ( 2.969333333333334490, 2.706666666666668331, -0.05833333333333418080 ) ) ;
#3145 = FACE_BOUND ( 'NONE', #2756, .T. ) ;
#3146 = CARTESIAN_POINT ( 'NONE',  ( -0.3119999999999999996, 0.5458333333333329485, -3.820898013339742174E-17 ) ) ;
#3147 = CARTESIAN_POINT ( 'NONE',  ( 0.3119999999999999996, 4.686194444444444329, 0.1292346314604056190 ) ) ;
#3148 = CC_DESIGN_PERSON_AND_ORGANIZATION_ASSIGNMENT ( #16989, #11388, ( #15678 ) ) ;
#3149 = CARTESIAN_POINT ( 'NONE',  ( -0.2819296736111110979, 4.293833333409199149, -0.1167790944451422980 ) ) ;
#3150 = DIRECTION ( 'NONE',  ( 0.000000000000000000, 0.000000000000000000, -1.000000000000000000 ) ) ;
#3151 = FACE_OUTER_BOUND ( 'NONE', #13925, .T. ) ;
#3152 = CARTESIAN_POINT ( 'NONE',  ( 0.2206173157302028232, 0.5180555554038226429, -0.2206173157302028232 ) ) ;
#3153 = CARTESIAN_POINT ( 'NONE',  ( 0.2209708691207961095, -0.2209708691207961651, -0.02277777777777661300 ) ) ;
#3154 = CARTESIAN_POINT ( 'NONE',  ( 5.178964085587577574E-17, 4.588972222298087544, 0.2819296736111110979 ) ) ;
#3155 = CARTESIAN_POINT ( 'NONE',  ( -0.2344453928311062418, 4.508576492912489186, 0.2058803838101449790 ) ) ;
#3156 = AXIS2_PLACEMENT_3D ( 'NONE', #1865, #1629, #9305 ) ;
#3157 = PERSON_AND_ORGANIZATION ( #15518, #2538 ) ;
#3158 = CARTESIAN_POINT ( 'NONE',  ( -0.07226797383944986997, -0.2674160455368901346, -0.06558227484231506088 ) ) ;
#3159 = CARTESIAN_POINT ( 'NONE',  ( 0.2764156081756483641, -0.1144950937579611167, 0.1126388888888909395 ) ) ;
#3160 = CARTESIAN_POINT ( 'NONE',  ( -0.1993543840281266910, 4.137583333409199149, -0.1993543840281266910 ) ) ;
#3161 = CARTESIAN_POINT ( 'NONE',  ( -0.001245755308147351035, 4.821647350372675334, -0.3119976684412342216 ) ) ;
#3162 = DIRECTION ( 'NONE',  ( 0.8320502943378438321, 0.4803844614152620873, -0.2773500981126135745 ) ) ;
#3163 = CARTESIAN_POINT ( 'NONE',  ( 0.2764156081756483641, -0.1144950937579611028, 0.1751388888888914530 ) ) ;
#3164 = CARTESIAN_POINT ( 'NONE',  ( -0.3613381517857144343, 0.1223214284738861207, 0.1174058825155740171 ) ) ;
#3165 = CARTESIAN_POINT ( 'NONE',  ( 1.726321361862525858E-17, 0.04930555547968892144, -0.2819296736111110979 ) ) ;
#3166 = CARTESIAN_POINT ( 'NONE',  ( 0.4687500000000002776, 0.2570931668155775895, 0.04874733047933993424 ) ) ;
#3167 = FACE_OUTER_BOUND ( 'NONE', #2935, .T. ) ;
#3168 = ADVANCED_FACE ( 'NONE', ( #23673 ), #6867, .T. ) ;
#3169 = CARTESIAN_POINT ( 'NONE',  ( -0.1918087731350874570, 0.2752783659658505355, -0.7250770848209401320 ) ) ;
#3170 = CARTESIAN_POINT ( 'NONE',  ( 0.2764156081756484196, -5.077672346800151106E-17, -0.05055555555555477781 ) ) ;
#3171 = CARTESIAN_POINT ( 'NONE',  ( 0.2230971623002954429, 0.2230971623002953319, 0.3747916666666706309 ) ) ;
#3172 = ORIENTED_EDGE ( 'NONE', *, *, #7936, .T. ) ;
#3173 = EDGE_LOOP ( 'NONE', ( #2490, #3556 ) ) ;
#3174 = DIRECTION ( 'NONE',  ( 0.000000000000000000, 0.000000000000000000, 1.000000000000000000 ) ) ;
#3175 = CARTESIAN_POINT ( 'NONE',  ( 0.3125000000000000000, -5.740531871003217465E-17, 0.03277777777777902274 ) ) ;
#3176 = CARTESIAN_POINT ( 'NONE',  ( 0.2819296736111110424, 0.4763888888130222710, 0.1167790944451424923 ) ) ;
#3177 = CARTESIAN_POINT ( 'NONE',  ( -0.1993543840281266355, 3.929250000075865668, 0.1993543840281267465 ) ) ;
#3178 = CARTESIAN_POINT ( 'NONE',  ( -7.726019084026502927E-17, 0.4446428569477723358, 0.4205848896953069405 ) ) ;
#3179 = EDGE_CURVE ( 'NONE', #21850, #23449, #13104, .T. ) ;
#3180 = CARTESIAN_POINT ( 'NONE',  ( -0.1167790944451423257, 4.356333333409199149, -0.2819296736111110424 ) ) ;
#3181 = CARTESIAN_POINT ( 'NONE',  ( 0.2661418463900624420, 5.135117573705075600, -0.1518351709947930450 ) ) ;
#3182 = FACE_OUTER_BOUND ( 'NONE', #4475, .T. ) ;
#3183 = VERTEX_POINT ( 'NONE', #12860 ) ;
#3184 = CARTESIAN_POINT ( 'NONE',  ( 5.731347020009612645E-17, 4.009111111111109516, 0.3119999999999999996 ) ) ;
#3185 = CARTESIAN_POINT ( 'NONE',  ( -0.2819296736111110424, 5.182722222298088433, -0.1167790944451423119 ) ) ;
#3186 = CARTESIAN_POINT ( 'NONE',  ( 0.2476760547999725393, 4.190764322939071640, 0.1908289239165902873 ) ) ;
#3187 = DIRECTION ( 'NONE',  ( -0.000000000000000000, -1.000000000000000000, -0.000000000000000000 ) ) ;
#3188 = CARTESIAN_POINT ( 'NONE',  ( -1.726321361862525858E-17, 4.894527777853642903, -0.2819296736111110979 ) ) ;
#3189 = DATE_TIME_ROLE ( 'classification_date' ) ;
#3190 = ORIENTED_EDGE ( 'NONE', *, *, #16584, .F. ) ;
#3191 = CARTESIAN_POINT ( 'NONE',  ( -0.1292346314604058410, 0.3270833331816004330, 0.3119999999999998885 ) ) ;
#3192 = EDGE_CURVE ( 'NONE', #13735, #7263, #18972, .T. ) ;
#3193 = CARTESIAN_POINT ( 'NONE',  ( -0.3009857094490465679, 4.555141368925776924, -0.09131701761149857433 ) ) ;
#3194 = ORIENTED_EDGE ( 'NONE', *, *, #2449, .F. ) ;
#3195 = CARTESIAN_POINT ( 'NONE',  ( 0.2819296736111110979, 0.2715277777019111660, 0.000000000000000000 ) ) ;
#3196 = ADVANCED_FACE ( 'NONE', ( #1622 ), #18625, .T. ) ;
#3197 = ORIENTED_EDGE ( 'NONE', *, *, #19594, .T. ) ;
#3198 = CARTESIAN_POINT ( 'NONE',  ( -0.2819296736111110424, 0.01805555547968892838, -0.1167790944451423396 ) ) ;
#3199 = CARTESIAN_POINT ( 'NONE',  ( 0.01875000000000005482, -0.5520911949125800744, 0.06112444011295372487 ) ) ;
#3200 = CARTESIAN_POINT ( 'NONE',  ( -0.5116234456863466562, 4.027014562472920112, 2.549370209580444691 ) ) ;
#3201 = CARTESIAN_POINT ( 'NONE',  ( 0.2472135954999579166, -0.03928571428571429880, 0.3402603233408160732 ) ) ;
#3202 = CARTESIAN_POINT ( 'NONE',  ( -0.2299564775410312401, 5.051042695534824212, -0.2131007688933645450 ) ) ;
#3203 = DIRECTION ( 'NONE',  ( 0.000000000000000000, 0.000000000000000000, -1.000000000000000000 ) ) ;
#3204 = DIRECTION ( 'NONE',  ( 0.000000000000000000, 0.000000000000000000, -1.000000000000000000 ) ) ;
#3205 = DIRECTION ( 'NONE',  ( -0.000000000000000000, -1.000000000000000000, -0.000000000000000000 ) ) ;
#3206 = CARTESIAN_POINT ( 'NONE',  ( -0.2819296736111110979, 4.477861111186976828, 0.000000000000000000 ) ) ;
#3207 = CARTESIAN_POINT ( 'NONE',  ( -0.3119999999999999996, 0.2611111109593781676, -3.820898013339742174E-17 ) ) ;
#3208 = ADVANCED_FACE ( 'NONE', ( #7173 ), #11198, .T. ) ;
#3209 = CARTESIAN_POINT ( 'NONE',  ( 0.2819296736111110979, 5.227861111186977716, -3.452642723725051716E-17 ) ) ;
#3210 = CARTESIAN_POINT ( 'NONE',  ( -0.01965242898639488894, 0.04348884421539742084, -0.2924957164008217814 ) ) ;
#3211 = CARTESIAN_POINT ( 'NONE',  ( 0.3007072963801942223, 3.754733255434872241, -0.08834097405045530926 ) ) ;
#3212 = LINE ( 'NONE', #8945, #20293 ) ;
#3213 = CARTESIAN_POINT ( 'NONE',  ( -0.06344583501299609629, 4.792058108258712146, 0.3056432983527924696 ) ) ;
#3214 = CARTESIAN_POINT ( 'NONE',  ( 0.2206173157302028787, 4.300777777929509327, 0.2206173157302027954 ) ) ;
#3215 = CARTESIAN_POINT ( 'NONE',  ( -0.2819296736111110424, 4.648000000075866112, 0.1167790944451424923 ) ) ;
#3216 =( BOUNDED_CURVE ( )  B_SPLINE_CURVE ( 2, ( #11876, #4414, #4174, #11750, #7947, #8187, #5879, #6366, #20641 ),
 .UNSPECIFIED., .F., .F. ) 
 B_SPLINE_CURVE_WITH_KNOTS ( ( 3, 2, 2, 2, 3 ),
 ( 0.3125000000000000555, 0.3229166666666667407, 0.3333333333333333703, 0.3437500000000000000, 0.3541666666666666852 ),
 .UNSPECIFIED. ) 
 CURVE ( )  GEOMETRIC_REPRESENTATION_ITEM ( )  RATIONAL_B_SPLINE_CURVE ( ( 0.9999999999999995559, 0.9238795325112871826, 1.000000000000000000, 0.9238795325112867385, 1.000000000000000000, 0.9238795325112867385, 1.000000000000000000, 0.9238795325112867385, 1.000000000000000000 ) ) 
 REPRESENTATION_ITEM ( '' )  );
#3217 = CARTESIAN_POINT ( 'NONE',  ( 0.2819296736111110979, 3.877166666742531742, 0.1167790944451422425 ) ) ;
#3218 = ORIENTED_EDGE ( 'NONE', *, *, #967, .F. ) ;
#3219 = AXIS2_PLACEMENT_3D ( 'NONE', #13395, #11567, #3123 ) ;
#3220 = ORIENTED_EDGE ( 'NONE', *, *, #6925, .F. ) ;
#3221 = EDGE_CURVE ( 'NONE', #2053, #19970, #1958, .T. ) ;
#3222 = PERSON_AND_ORGANIZATION ( #15518, #2538 ) ;
#3223 = DIRECTION ( 'NONE',  ( -0.000000000000000000, -1.000000000000000000, -0.000000000000000000 ) ) ;
#3224 = FACE_OUTER_BOUND ( 'NONE', #23814, .T. ) ;
#3225 = ORIENTED_EDGE ( 'NONE', *, *, #2178, .T. ) ;
#3226 = CARTESIAN_POINT ( 'NONE',  ( -0.2206173157302028787, 0.2124999998482670627, 0.2206173157302027954 ) ) ;
#3227 = CARTESIAN_POINT ( 'NONE',  ( -0.009913296964756498908, 4.377433935782568675, -0.3118490548042810451 ) ) ;
#3228 = CARTESIAN_POINT ( 'NONE',  ( -0.5116234456863466562, -0.003009961218012348859, 2.549370209580444246 ) ) ;
#3229 = CARTESIAN_POINT ( 'NONE',  ( 0.1080314883215018618, 0.1837960933690710730, -0.7422718097737546206 ) ) ;
#3230 = ORIENTED_EDGE ( 'NONE', *, *, #2836, .F. ) ;
#3231 = CYLINDRICAL_SURFACE ( 'NONE', #4887, 0.3119999999999999996 ) ;
#3232 = CARTESIAN_POINT ( 'NONE',  ( -0.2819296736111110979, 0.2298611110352444808, -3.452642723725051716E-17 ) ) ;
#3233 = CARTESIAN_POINT ( 'NONE',  ( -0.1144950937579609918, -0.2764156081756484196, 0.3765277777777820134 ) ) ;
#3234 = B_SPLINE_CURVE_WITH_KNOTS ( 'NONE', 3,
 ( #20599, #18528, #353, #3896, #5840, #1818, #11340, #7673, #7794, #20481, #18769, #9505 ),
 .UNSPECIFIED., .F., .F.,
 ( 4, 2, 2, 2, 2, 4 ),
 ( 0.000000000000000000, 0.003345931539952399971, 0.005018897309928598005, 0.006691863079904796473, 0.01003779461985718907, 0.01338372615980958427 ),
 .UNSPECIFIED. ) ;
#3235 = VERTEX_POINT ( 'NONE', #20338 ) ;
#3236 = VECTOR ( 'NONE', #1118, 39.37007874015748854 ) ;
#3237 = EDGE_CURVE ( 'NONE', #8054, #8072, #7415, .T. ) ;
#3238 = CARTESIAN_POINT ( 'NONE',  ( -0.1167790944451423257, 4.342444444520310753, -0.2819296736111110424 ) ) ;
#3239 = CARTESIAN_POINT ( 'NONE',  ( 0.2206173157302028232, 0.1916666666666663466, -0.2206173157302028232 ) ) ;
#3240 = DIRECTION ( 'NONE',  ( 8.659560562354932858E-17, 0.7071067811865474617, -0.7071067811865474617 ) ) ;
#3241 = CARTESIAN_POINT ( 'NONE',  ( -0.08757809820678906509, 4.235785868357317518, 0.3004240109509383472 ) ) ;
#3242 = CARTESIAN_POINT ( 'NONE',  ( 0.3119999999999999996, 4.082027777777776478, -0.1292346314604056745 ) ) ;
#3243 = CARTESIAN_POINT ( 'NONE',  ( 0.2206173157302028787, 4.856333333485065573, 0.2206173157302027954 ) ) ;
#3244 = ORIENTED_EDGE ( 'NONE', *, *, #22173, .F. ) ;
#3245 = FACE_OUTER_BOUND ( 'NONE', #23069, .T. ) ;
#3246 = ORIENTED_EDGE ( 'NONE', *, *, #68, .T. ) ;
#3247 = CARTESIAN_POINT ( 'NONE',  ( -0.1426465030096581710, 4.881379615490812007, -0.2780736469684209622 ) ) ;
#3248 = VECTOR ( 'NONE', #10828, 39.37007874015748854 ) ;
#3249 = CARTESIAN_POINT ( 'NONE',  ( 0.1306872919485616846, 0.3155070326520292290, 0.2150694444444475051 ) ) ;
#3250 = CARTESIAN_POINT ( 'NONE',  ( -0.1116596296178200276, 0.4187499999024575370, 0.3436530038418508792 ) ) ;
#3251 = CARTESIAN_POINT ( 'NONE',  ( 0.03741580292204597924, -0.5077710590216990560, 0.4064395341356261682 ) ) ;
#3252 = CARTESIAN_POINT ( 'NONE',  ( 0.3613381517857143232, 0.1401785713310289838, -0.1174058825155740587 ) ) ;
#3253 = CARTESIAN_POINT ( 'NONE',  ( -0.1167790944451424506, 0.1986111110352444808, 0.2819296736111110424 ) ) ;
#3254 = CARTESIAN_POINT ( 'NONE',  ( -0.2764156081756484196, -0.1144950937579609362, 0.04319444444444596465 ) ) ;
#3255 = CARTESIAN_POINT ( 'NONE',  ( 0.1167790944451422702, 5.127166666742532186, -0.2819296736111110424 ) ) ;
#3256 = CARTESIAN_POINT ( 'NONE',  ( 0.2295400061202557962, 4.481090041848301730, -0.2126894043619363961 ) ) ;
#3257 = ORIENTED_EDGE ( 'NONE', *, *, #21842, .F. ) ;
#3258 = EDGE_CURVE ( 'NONE', #20894, #6009, #6178, .T. ) ;
#3259 = CARTESIAN_POINT ( 'NONE',  ( -7.000945310522701902E-17, 0.2303571426620580065, 0.3999999999999999667 ) ) ;
#3260 = CARTESIAN_POINT ( 'NONE',  ( -0.01726427071093490639, 4.293343159678996379, 0.3115899811169826616 ) ) ;
#3261 = CARTESIAN_POINT ( 'NONE',  ( -0.4593750000000003664, -6.734002413227273428E-17, 0.4343810118395207698 ) ) ;
#3262 = CARTESIAN_POINT ( 'NONE',  ( 0.2206173157302028232, 0.5805555555555552694, -0.2206173157302028232 ) ) ;
#3263 = CARTESIAN_POINT ( 'NONE',  ( -0.1292346314604056745, 4.707027777777777366, -0.3119999999999999996 ) ) ;
#3264 = CARTESIAN_POINT ( 'NONE',  ( -0.1167790944451423119, 3.898000000075865223, -0.2819296736111110979 ) ) ;
#3265 = CIRCLE ( 'NONE', #156, 0.01875000000000000625 ) ;
#3266 = CARTESIAN_POINT ( 'NONE',  ( 0.1993543840281266633, 3.845916666742533074, -0.1993543840281266910 ) ) ;
#3267 = CARTESIAN_POINT ( 'NONE',  ( -0.1236067977499789583, 0.2071428571428570731, -0.3804226065180614791 ) ) ;
#3268 = CARTESIAN_POINT ( 'NONE',  ( -5.731347020009612645E-17, 0.4972222220704892726, 0.3119999999999999996 ) ) ;
#3269 = EDGE_LOOP ( 'NONE', ( #6569, #418, #1170, #13342 ) ) ;
#3270 = CARTESIAN_POINT ( 'NONE',  ( -0.2209708691207961373, -0.2209708691207961095, 0.1230555555555574998 ) ) ;
#3271 = CARTESIAN_POINT ( 'NONE',  ( -0.1993543840281266910, 4.568138888964754507, -0.1993543840281266910 ) ) ;
#3272 = CARTESIAN_POINT ( 'NONE',  ( -0.02174346296206112333, 4.488903266706190109, -0.3112889508319767740 ) ) ;
#3273 = CALENDAR_DATE ( 2026, 7, 10 ) ;
#3274 = DIRECTION ( 'NONE',  ( 0.000000000000000000, 0.000000000000000000, -1.000000000000000000 ) ) ;
#3275 = CARTESIAN_POINT ( 'NONE',  ( 0.2764156081756483641, 0.1144950937579610056, 0.2862500000000035016 ) ) ;
#3276 = B_SPLINE_CURVE_WITH_KNOTS ( 'NONE', 3,
 ( #9465, #5441, #10941, #1903, #9227, #3606, #7277, #13025, #11182, #18730, #16898, #18369, #16664, #20440, #14960, #24087, #5683, #22380, #2026, #11059, #9346, #18489, #22022, #7397, #14849, #16787 ),
 .UNSPECIFIED., .F., .F.,
 ( 4, 2, 2, 2, 2, 2, 2, 2, 2, 2, 2, 2, 4 ),
 ( 0.02660920303947646864, 0.02748246392853086195, 0.02835572481758525526, 0.03010224659569404188, 0.03097550748474843518, 0.03184876837380282849, 0.03272202926285722180, 0.03359529015191161511, 0.03534181193002039478, 0.03708833370812918140, 0.03796159459718358165, 0.03883485548623796801, 0.04058137726434675463 ),
 .UNSPECIFIED. ) ;
#3277 = CARTESIAN_POINT ( 'NONE',  ( 0.1167790944451422702, 4.071611111186977716, -0.2819296736111110979 ) ) ;
#3278 = CONICAL_SURFACE ( 'NONE', #8329, 1.243000000000000105, 0.2617993877991500740 ) ;
#3279 = CARTESIAN_POINT ( 'NONE',  ( 0.3124999999999996669, 0.1294417382415925521, -0.07486111111111071192 ) ) ;
#3280 = CARTESIAN_POINT ( 'NONE',  ( 0.01995244822899069209, 5.161835221482045988, -0.2985861170655538799 ) ) ;
#3281 = CARTESIAN_POINT ( 'NONE',  ( 0.4235215514428773420, 2.693521551442877193, -0.6521195261172616497 ) ) ;
#3282 = CARTESIAN_POINT ( 'NONE',  ( -0.1116596296178199582, -0.03839285724039953607, -0.3436530038418508792 ) ) ;
#3283 = CARTESIAN_POINT ( 'NONE',  ( 0.2819296736111110979, 0.03541666659080003332, 0.000000000000000000 ) ) ;
#3284 = CARTESIAN_POINT ( 'NONE',  ( 0.4795759056698289946, 0.04342265654436765904, 0.07439901873394898224 ) ) ;
#3285 = CARTESIAN_POINT ( 'NONE',  ( 0.1236067977499789028, 0.01964285694777234345, 0.3804226065180614791 ) ) ;
#3286 = CARTESIAN_POINT ( 'NONE',  ( -0.1989242110943551245, 0.4407889530968281400, -0.7231588590637065828 ) ) ;
#3287 = CARTESIAN_POINT ( 'NONE',  ( -0.2764156081756484196, -0.1144950937579609362, 0.09180555555555744429 ) ) ;
#3288 = CARTESIAN_POINT ( 'NONE',  ( -0.2764156081756484196, 0.1144950937579609918, 0.03625000000000144079 ) ) ;
#3289 = VERTEX_POINT ( 'NONE', #16683 ) ;
#3290 = ORIENTED_EDGE ( 'NONE', *, *, #19171, .F. ) ;
#3291 = FACE_OUTER_BOUND ( 'NONE', #3269, .T. ) ;
#3292 = CARTESIAN_POINT ( 'NONE',  ( 7.459700445346810805E-07, 4.043833313442511290, -0.3119999999991081574 ) ) ;
#3293 = CARTESIAN_POINT ( 'NONE',  ( -0.3119999999999999996, -0.006250000000000336016, 0.1292346314604056190 ) ) ;
#3294 = CARTESIAN_POINT ( 'NONE',  ( -0.1993543840281266910, 3.859805555631421470, -0.1993543840281266910 ) ) ;
#3295 = CARTESIAN_POINT ( 'NONE',  ( -0.1116596296178199582, 0.1044642856167433131, -0.3436530038418508792 ) ) ;
#3296 = CARTESIAN_POINT ( 'NONE',  ( 0.1993543840281266633, 4.457027777853643791, -0.1993543840281266910 ) ) ;
#3297 = PRODUCT_DEFINITION_SHAPE ( 'NONE', 'NONE',  #21185 ) ;
#3298 = FACE_OUTER_BOUND ( 'NONE', #6519, .T. ) ;
#3299 = DIRECTION ( 'NONE',  ( 0.4999999999999916178, 6.654928120984803295E-16, 0.8660254037844433705 ) ) ;
#3300 = ORIENTED_EDGE ( 'NONE', *, *, #11112, .F. ) ;
#3301 = CARTESIAN_POINT ( 'NONE',  ( 0.1915320766489893856, 4.355118862228665400, 0.2496463631673534467 ) ) ;
#3302 = CARTESIAN_POINT ( 'NONE',  ( -0.1167790944451423257, 5.175777777853644679, -0.2819296736111110424 ) ) ;
#3303 = CARTESIAN_POINT ( 'NONE',  ( 0.2335926053540489100, 4.203040725598064853, -0.2068301295312730270 ) ) ;
#3304 = B_SPLINE_CURVE_WITH_KNOTS ( 'NONE', 3,
 ( #22158, #20334, #211, #14977, #20456, #11437 ),
 .UNSPECIFIED., .F., .F.,
 ( 4, 2, 4 ),
 ( 0.000000000000000000, 0.003402024485550936284, 0.006804048971101872567 ),
 .UNSPECIFIED. ) ;
#3305 = EDGE_CURVE ( 'NONE', #7226, #12971, #6944, .T. ) ;
#3306 = APPROVAL_PERSON_ORGANIZATION ( #1247, #13608, #23421 ) ;
#3307 = CARTESIAN_POINT ( 'NONE',  ( -0.1993543840281266355, 4.804250000075865223, 0.1993543840281267465 ) ) ;
#3308 = CALENDAR_DATE ( 2026, 7, 10 ) ;
#3309 = ORIENTED_EDGE ( 'NONE', *, *, #68, .F. ) ;
#3310 = EDGE_CURVE ( 'NONE', #13148, #21887, #1798, .T. ) ;
#3311 = CARTESIAN_POINT ( 'NONE',  ( -0.3120000000000000551, 0.3201388887371559577, 0.1292346314604056190 ) ) ;
#3312 = CARTESIAN_POINT ( 'NONE',  ( 2.320391506243691726, 2.740000000000000213, -2.452934640057647719 ) ) ;
#3313 = EDGE_LOOP ( 'NONE', ( #9399, #16060, #19784, #5093 ) ) ;
#3314 = CARTESIAN_POINT ( 'NONE',  ( 0.2819296736111110424, 0.2194444443685777957, -0.1167790944451423119 ) ) ;
#3315 = CARTESIAN_POINT ( 'NONE',  ( 0.2819296736111110424, -0.002777777853644409004, -0.1167790944451423119 ) ) ;
#3316 = CARTESIAN_POINT ( 'NONE',  ( 0.000000000000000000, 5.384999999999999787, 0.000000000000000000 ) ) ;
#3317 = DIRECTION ( 'NONE',  ( 0.8660254037844361541, 0.000000000000000000, 0.5000000000000042188 ) ) ;
#3318 = AXIS2_PLACEMENT_3D ( 'NONE', #13654, #20832, #2425 ) ;
#3319 = CARTESIAN_POINT ( 'NONE',  ( -0.4000000000000000222, -0.06071428571428573451, 0.1299678784931624920 ) ) ;
#3320 = CARTESIAN_POINT ( 'NONE',  ( 5.731347020009612645E-17, 4.509111111111110404, 0.3119999999999999996 ) ) ;
#3321 = CARTESIAN_POINT ( 'NONE',  ( 5.731347020009612645E-17, 4.175777777777776478, 0.3119999999999999996 ) ) ;
#3322 = CARTESIAN_POINT ( 'NONE',  ( -0.02020282852508829483, 3.877718746106461278, -0.3119025878752364478 ) ) ;
#3323 = DIRECTION ( 'NONE',  ( -0.000000000000000000, 1.000000000000000000, -0.000000000000000000 ) ) ;
#3324 = CARTESIAN_POINT ( 'NONE',  ( 0.1993543840281266633, 4.401472222298088433, -0.1993543840281266910 ) ) ;
#3325 = PLANE ( 'NONE',  #8132 ) ;
#3326 = LINE ( 'NONE', #18569, #12188 ) ;
#3327 = CARTESIAN_POINT ( 'NONE',  ( -0.2819296736111110979, 5.033416666742532186, 0.000000000000000000 ) ) ;
#3328 = CARTESIAN_POINT ( 'NONE',  ( -0.3011022955695156211, 0.05170836598878657958, -0.01273678397337616591 ) ) ;
#3329 = CARTESIAN_POINT ( 'NONE',  ( 2.570936052289255124E-07, 3.738287934957344127, 0.3119999999997750129 ) ) ;
#3330 = LOCAL_TIME ( 21, 9, 13.00000000000000000, #794 ) ;
#3331 = CARTESIAN_POINT ( 'NONE',  ( 0.06877731076760502937, 0.04436119539538452977, 0.2860349230690588107 ) ) ;
#3332 = DIRECTION ( 'NONE',  ( -0.000000000000000000, -0.000000000000000000, -1.000000000000000000 ) ) ;
#3333 = CARTESIAN_POINT ( 'NONE',  ( -1.910449006669871087E-17, 4.377166666818398610, -0.3119999999999999996 ) ) ;
#3334 = CARTESIAN_POINT ( 'NONE',  ( -0.1167790944451423535, 4.488277777853643791, 0.2819296736111110979 ) ) ;
#3335 = B_SPLINE_CURVE_WITH_KNOTS ( 'NONE', 3,
 ( #15236, #11585, #17184, #13768, #21075, #591, #8260, #22665, #22547, #21194, #15592, #20957, #13301 ),
 .UNSPECIFIED., .F., .F.,
 ( 4, 2, 2, 2, 1, 2, 4 ),
 ( 0.000000000000000000, 0.001498478264507173679, 0.002996956529014346490, 0.003746195661267932679, 0.004495434793521518868, 0.005244673925775105057, 0.005993913058028690378 ),
 .UNSPECIFIED. ) ;
#3336 = CARTESIAN_POINT ( 'NONE',  ( -0.1993543840281266910, 3.901472222298087544, -0.1993543840281266910 ) ) ;
#3337 = ORIENTED_EDGE ( 'NONE', *, *, #17335, .T. ) ;
#3338 = AXIS2_PLACEMENT_3D ( 'NONE', #18171, #7079, #1467 ) ;
#3339 = ORIENTED_EDGE ( 'NONE', *, *, #643, .F. ) ;
#3340 = VERTEX_POINT ( 'NONE', #5207 ) ;
#3341 = COORDINATED_UNIVERSAL_TIME_OFFSET ( 0, 0, .AHEAD. ) ;
#3342 = CARTESIAN_POINT ( 'NONE',  ( -0.1031051051773897304, -0.2870977370809309481, 0.4162540920893169072 ) ) ;
#3343 = EDGE_CURVE ( 'NONE', #11560, #8700, #7354, .T. ) ;
#3344 = CARTESIAN_POINT ( 'NONE',  ( -0.2727962046151662934, 4.942087318129531504, -0.1568363485577166649 ) ) ;
#3345 = CARTESIAN_POINT ( 'NONE',  ( 1.910449006669871087E-17, 0.3652777777777774237, -0.3119999999999999996 ) ) ;
#3346 = CC_DESIGN_SECURITY_CLASSIFICATION ( #12722, ( #8009 ) ) ;
#3347 = ORIENTED_EDGE ( 'NONE', *, *, #18731, .F. ) ;
#3348 = CARTESIAN_POINT ( 'NONE',  ( 0.3119999999999999996, 0.3444444442927114824, 0.000000000000000000 ) ) ;
#3349 = CARTESIAN_POINT ( 'NONE',  ( -0.2263603714153657742, 4.384333806754304064, -0.2147221485470059144 ) ) ;
#3350 = CARTESIAN_POINT ( 'NONE',  ( -0.2115755794123815592, 5.122769419632757781, 0.2240629809752085200 ) ) ;
#3351 = CARTESIAN_POINT ( 'NONE',  ( -0.1292346314604058410, 0.2784722222222218435, 0.3119999999999998885 ) ) ;
#3352 = CARTESIAN_POINT ( 'NONE',  ( -0.4000000000000000222, 0.3642857142857142128, -4.898587196589413075E-17 ) ) ;
#3353 = ORIENTED_EDGE ( 'NONE', *, *, #10794, .T. ) ;
#3354 = AXIS2_PLACEMENT_3D ( 'NONE', #615, #5620, #9523 ) ;
#3355 = CARTESIAN_POINT ( 'NONE',  ( 0.3080438441126990279, 5.084176856567461655, 0.05194822647866765425 ) ) ;
#3356 = CARTESIAN_POINT ( 'NONE',  ( -0.2764156081756484196, -0.1144950937579609362, 0.2584722222222254340 ) ) ;
#3357 = B_SPLINE_CURVE_WITH_KNOTS ( 'NONE', 3,
 ( #6404, #6523, #19450, #22979, #8225, #1039 ),
 .UNSPECIFIED., .F., .F.,
 ( 4, 2, 4 ),
 ( 0.006847393025867874912, 0.01026280280047527083, 0.01367821257508266761 ),
 .UNSPECIFIED. ) ;
#3358 = CARTESIAN_POINT ( 'NONE',  ( 0.2819296736111110424, 4.217444444520310753, -0.1167790944451423396 ) ) ;
#3359 = CARTESIAN_POINT ( 'NONE',  ( -0.1167790944451423535, 5.085500000075866112, 0.2819296736111110979 ) ) ;
#3360 = EDGE_CURVE ( 'NONE', #2823, #10167, #1921, .T. ) ;
#3361 = CARTESIAN_POINT ( 'NONE',  ( -0.4687500000000004441, -0.2170120125989246918, 0.07051005015414456290 ) ) ;
#3362 = CARTESIAN_POINT ( 'NONE',  ( -0.2612101927628759923, 4.229576235931883588, 0.1754577556920814685 ) ) ;
#3363 = CARTESIAN_POINT ( 'NONE',  ( 5.731347020009612645E-17, 4.120222222222221120, 0.3119999999999999996 ) ) ;
#3364 = CARTESIAN_POINT ( 'NONE',  ( 0.2206173157302028787, 4.967444444596176290, 0.2206173157302027954 ) ) ;
#3365 = CARTESIAN_POINT ( 'NONE',  ( 0.2943229328651665866, 4.810734450191622713, -0.1059385550757641070 ) ) ;
#3366 = EDGE_CURVE ( 'NONE', #7614, #17116, #13459, .T. ) ;
#3367 = ADVANCED_FACE ( 'NONE', ( #20700 ), #15337, .F. ) ;
#3368 = ADVANCED_FACE ( 'NONE', ( #3990 ), #17166, .T. ) ;
#3369 = CARTESIAN_POINT ( 'NONE',  ( -0.1294417382415922191, 0.3125000000000000000, 0.2168055555555583047 ) ) ;
#3370 = ORIENTED_EDGE ( 'NONE', *, *, #7090, .T. ) ;
#3371 = CARTESIAN_POINT ( 'NONE',  ( -0.3039836006089354226, 4.888818180532651603, -0.08126209352896139604 ) ) ;
#3372 = EDGE_CURVE ( 'NONE', #19011, #4071, #18995, .T. ) ;
#3373 = CARTESIAN_POINT ( 'NONE',  ( 0.3155070326520292290, 0.1306872919485615736, 0.2081250000000030298 ) ) ;
#3374 = CARTESIAN_POINT ( 'NONE',  ( 0.2233192592356399164, 0.3580357141881718164, 0.3073725909049500604 ) ) ;
#3375 = CARTESIAN_POINT ( 'NONE',  ( 0.3075813148943679631, -0.3526675668868561875, 0.4297318021118050058 ) ) ;
#3376 = LINE ( 'NONE', #21906, #3248 ) ;
#3377 = CARTESIAN_POINT ( 'NONE',  ( 0.2819296736111110979, 0.2749999999241334314, -0.1167790944451422980 ) ) ;
#3378 = CARTESIAN_POINT ( 'NONE',  ( 0.2764156081756483641, -0.1144950937579611167, 0.1751388888888914530 ) ) ;
#3379 = CARTESIAN_POINT ( 'NONE',  ( 0.1167790944451422702, 5.182722222298088433, -0.2819296736111110424 ) ) ;
#3380 = DIRECTION ( 'NONE',  ( -0.000000000000000000, -1.000000000000000000, -0.000000000000000000 ) ) ;
#3381 = VERTEX_POINT ( 'NONE', #13165 ) ;
#3382 = CARTESIAN_POINT ( 'NONE',  ( -0.0001469343572505705023, 3.766059503595236446, -0.3119999755966755828 ) ) ;
#3383 = CARTESIAN_POINT ( 'NONE',  ( 0.1292346314604031765, 3.866750000000000131, -0.3120000000000024420 ) ) ;
#3384 = CARTESIAN_POINT ( 'NONE',  ( 0.1128137788402567426, 4.873987063709920520, -0.2914807742742103192 ) ) ;
#3385 = CARTESIAN_POINT ( 'NONE',  ( 5.731347020009612645E-17, 4.564666666666665762, 0.3119999999999999996 ) ) ;
#3386 = CARTESIAN_POINT ( 'NONE',  ( 0.3125000000000000000, -5.740531871003217465E-17, 0.3105555555555590819 ) ) ;
#3387 = CARTESIAN_POINT ( 'NONE',  ( -0.2206173157302027676, 4.835499999999999687, 0.2206173157302028787 ) ) ;
#3388 = AXIS2_PLACEMENT_3D ( 'NONE', #12973, #20390, #7460 ) ;
#3389 = CARTESIAN_POINT ( 'NONE',  ( 0.1993543840281267465, 4.095916666742532186, 0.1993543840281266633 ) ) ;
#3390 = CARTESIAN_POINT ( 'NONE',  ( -1.726321361862525858E-17, 3.797305555631421470, -0.2819296736111110979 ) ) ;
#3391 = CARTESIAN_POINT ( 'NONE',  ( 0.2100805295423999741, 4.037387642597302317, -0.2317816973857660945 ) ) ;
#3392 = CARTESIAN_POINT ( 'NONE',  ( -0.1060554323913586589, -0.003009961218012348859, 2.783525011231007706 ) ) ;
#3393 = B_SPLINE_CURVE_WITH_KNOTS ( 'NONE', 3,
 ( #15864, #1559, #987, #8416, #17818, #23048, #2700, #23280, #6594, #22935, #2587, #14042, #12228, #8176, #1108, #10835, #5202, #8542, #10152, #21237, #15984, #6356, #23405, #11990, #866, #6713, #14158, #3382, #18263, #6231 ),
 .UNSPECIFIED., .F., .F.,
 ( 4, 2, 2, 2, 2, 2, 2, 2, 2, 2, 1, 1, 1, 1, 1, 1, 2, 4 ),
 ( 0.9411639604301500484, 0.9434483960034079075, 0.9457328315766656557, 0.9480172671499235149, 0.9503017027231813740, 0.9525861382964391222, 0.9548705738696969814, 0.9571550094429547295, 0.9582972272295836591, 0.9588683361228981239, 0.9591538905695553563, 0.9592966677928840280, 0.9593680564045482528, 0.9594037507103804208, 0.9594215978632965047, 0.9594305214397546022, 0.9594349832279835955, 0.9594394450162125887 ),
 .UNSPECIFIED. ) ;
#3394 = ORIENTED_EDGE ( 'NONE', *, *, #85, .T. ) ;
#3395 = CARTESIAN_POINT ( 'NONE',  ( 0.3125000000000000000, -5.740531871003217465E-17, 0.1438888888888910089 ) ) ;
#3396 = ORIENTED_EDGE ( 'NONE', *, *, #23175, .T. ) ;
#3397 = CARTESIAN_POINT ( 'NONE',  ( -0.1167790944451423257, 4.509111111186976828, -0.2819296736111110424 ) ) ;
#3398 = CARTESIAN_POINT ( 'NONE',  ( 0.2206173157302028787, 3.793833333333332725, 0.2206173157302027954 ) ) ;
#3399 = EDGE_CURVE ( 'NONE', #8579, #7867, #2174, .T. ) ;
#3400 = CARTESIAN_POINT ( 'NONE',  ( -0.1309139991618845367, -0.2436136748879068614, -0.06558227484231496374 ) ) ;
#3401 = CARTESIAN_POINT ( 'NONE',  ( -0.2764156081756484196, -0.1144950937579609362, 0.2584722222222254340 ) ) ;
#3402 = CIRCLE ( 'NONE', #10425, 0.7700000000000013500 ) ;
#3403 = CARTESIAN_POINT ( 'NONE',  ( 0.1993543840281266633, 3.790361111186977272, -0.1993543840281266910 ) ) ;
#3404 = CARTESIAN_POINT ( 'NONE',  ( -8.183246661411124563E-08, 3.960496777434589610, 0.3119999999999772400 ) ) ;
#3405 = CARTESIAN_POINT ( 'NONE',  ( 0.1347543868356496644, 5.157564342225265719, -0.2691372244021535964 ) ) ;
#3406 = CARTESIAN_POINT ( 'NONE',  ( 0.1954553509668047195, 0.1954553509668046085, 0.3522222222222262111 ) ) ;
#3407 = CARTESIAN_POINT ( 'NONE',  ( 0.2923287055106771337, -0.05267857152611382654, -0.2123892367102620249 ) ) ;
#3408 = CARTESIAN_POINT ( 'NONE',  ( 0.2819296736111110424, 0.3652777777019111105, 0.1167790944451424923 ) ) ;
#3409 = CARTESIAN_POINT ( 'NONE',  ( -0.5116234456863258950, 4.111524471938507119, -2.845780280100676851 ) ) ;
#3410 = LINE ( 'NONE', #5482, #13147 ) ;
#3411 = CARTESIAN_POINT ( 'NONE',  ( -0.1236081594474160439, 0.5483826904852967532, -0.7397659828179361519 ) ) ;
#3412 = CARTESIAN_POINT ( 'NONE',  ( 0.1954553509668047195, 0.1954553509668046085, 0.01194444444444571485 ) ) ;
#3413 = CARTESIAN_POINT ( 'NONE',  ( -0.2764156081756484196, -0.1144950937579609362, -0.06791666666666604235 ) ) ;
#3414 = ORIENTED_EDGE ( 'NONE', *, *, #23741, .F. ) ;
#3415 = ORIENTED_EDGE ( 'NONE', *, *, #5906, .F. ) ;
#3416 = CARTESIAN_POINT ( 'NONE',  ( 0.2020650928029222304, 0.4371048157571743031, 0.07438423612653367878 ) ) ;
#3417 = CARTESIAN_POINT ( 'NONE',  ( 0.4687500000000002776, 0.04423121237726190119, 0.4171966076993701145 ) ) ;
#3418 = CARTESIAN_POINT ( 'NONE',  ( -5.731347020009612645E-17, 0.05972222222222188515, 0.3119999999999999996 ) ) ;
#3419 = CARTESIAN_POINT ( 'NONE',  ( -0.2819296736111110424, 3.807722222298089321, -0.1167790944451423119 ) ) ;
#3420 = CARTESIAN_POINT ( 'NONE',  ( 0.2923287055106771337, 0.2901785713310289783, 0.2123892367102621359 ) ) ;
#3421 = CARTESIAN_POINT ( 'NONE',  ( -0.2819296736111110424, 4.481333333409199149, 0.1167790944451424923 ) ) ;
#3422 = FACE_OUTER_BOUND ( 'NONE', #22090, .T. ) ;
#3423 = CARTESIAN_POINT ( 'NONE',  ( -0.2206173157302028232, 4.377166666666665762, -0.2206173157302028232 ) ) ;
#3424 = ORIENTED_EDGE ( 'NONE', *, *, #2601, .T. ) ;
#3425 = AXIS2_PLACEMENT_3D ( 'NONE', #10007, #23026, #6327 ) ;
#3426 = CARTESIAN_POINT ( 'NONE',  ( 0.3120000000000000551, 4.686194444444444329, 0.1292346314604056190 ) ) ;
#3427 = CARTESIAN_POINT ( 'NONE',  ( 0.1167790944451422702, 5.113277777853642903, -0.2819296736111110424 ) ) ;
#3428 = CARTESIAN_POINT ( 'NONE',  ( 0.2354754176334847293, 4.202962126866166770, -0.2046859565788392565 ) ) ;
#3429 = CARTESIAN_POINT ( 'NONE',  ( 0.06335377612981443751, 0.2321876527173024896, 0.4000000000000000222 ) ) ;
#3430 = CARTESIAN_POINT ( 'NONE',  ( 0.2819296736111111534, 4.654944444520309865, 0.1167790944451422563 ) ) ;
#3431 = CONTEXT_DEPENDENT_SHAPE_REPRESENTATION ( #4216, #23720 ) ;
#3432 = CARTESIAN_POINT ( 'NONE',  ( -0.1196036944483439418, 4.068140768160333209, 0.2893420950190842000 ) ) ;
#3433 = DIRECTION ( 'NONE',  ( -0.000000000000000000, -1.000000000000000000, -0.000000000000000000 ) ) ;
#3434 = ORIENTED_EDGE ( 'NONE', *, *, #20904, .F. ) ;
#3435 = CARTESIAN_POINT ( 'NONE',  ( -0.1167790944451424368, 0.3097222221463555303, 0.2819296736111110424 ) ) ;
#3436 = AXIS2_PLACEMENT_3D ( 'NONE', #4806, #19813, #10318 ) ;
#3437 = VERTEX_POINT ( 'NONE', #9485 ) ;
#3438 = CARTESIAN_POINT ( 'NONE',  ( -0.2819296736111110424, 0.2402777777019111938, -0.1167790944451423396 ) ) ;
#3439 = CYLINDRICAL_SURFACE ( 'NONE', #13509, 0.3119999999999999996 ) ;
#3440 = CARTESIAN_POINT ( 'NONE',  ( -0.2258351564880545503, 5.196761101924514570, -0.1766745448178271560 ) ) ;
#3441 = CARTESIAN_POINT ( 'NONE',  ( 0.2923287055106771337, 0.4151785713310289228, 0.2123892367102621359 ) ) ;
#3442 = CARTESIAN_POINT ( 'NONE',  ( 0.3155070326520292290, -0.1306872919485616569, -0.02451388888888812734 ) ) ;
#3443 = PLANE ( 'NONE',  #15739 ) ;
#3444 = ADVANCED_FACE ( 'NONE', ( #22525 ), #7772, .T. ) ;
#3445 = CARTESIAN_POINT ( 'NONE',  ( 0.2819296736111110979, 0.09097222214635558579, 0.000000000000000000 ) ) ;
#3446 = CARTESIAN_POINT ( 'NONE',  ( 5.178964085587577574E-17, 4.491750000075866112, 0.2819296736111110979 ) ) ;
#3447 = DIRECTION ( 'NONE',  ( -0.000000000000000000, -1.000000000000000000, -0.000000000000000000 ) ) ;
#3448 = CARTESIAN_POINT ( 'NONE',  ( 0.03357672467717862097, 4.542878599828895858, -0.3103008995289400218 ) ) ;
#3449 = CARTESIAN_POINT ( 'NONE',  ( 0.1993543840281266633, 5.068138888964754507, -0.1993543840281266910 ) ) ;
#3450 = CARTESIAN_POINT ( 'NONE',  ( 0.4687500000000003886, 0.1740113748017593776, 0.07813285960791813145 ) ) ;
#3451 = CARTESIAN_POINT ( 'NONE',  ( 0.2062776401250031866, 3.759720860179437629, -0.2349803605453861244 ) ) ;
#3452 = CARTESIAN_POINT ( 'NONE',  ( -0.07527472113052315061, 0.4862786960646409140, 0.4165495381634259364 ) ) ;
#3453 = CARTESIAN_POINT ( 'NONE',  ( -0.1650087075157100902, 0.4586159948670857078, 0.07156199457777139006 ) ) ;
#3454 = APPROVAL ( #10765, 'UNKNOWN' ) ;
#3455 = CARTESIAN_POINT ( 'NONE',  ( 0.1292346314604056190, 4.373694444596176290, -0.3119999999999999996 ) ) ;
#3456 = EDGE_CURVE ( 'NONE', #15771, #1725, #8758, .T. ) ;
#3457 = CARTESIAN_POINT ( 'NONE',  ( 5.178964085587577574E-17, 4.602861111186976828, 0.2819296736111110979 ) ) ;
#3458 = CARTESIAN_POINT ( 'NONE',  ( -0.2819296736111110424, 3.793833333409199149, -0.1167790944451423119 ) ) ;
#3459 = AXIS2_PLACEMENT_3D ( 'NONE', #7222, #1612, #9409 ) ;
#3460 = VERTEX_POINT ( 'NONE', #16917 ) ;
#3461 = ORIENTED_EDGE ( 'NONE', *, *, #12779, .F. ) ;
#3462 = ORIENTED_EDGE ( 'NONE', *, *, #16584, .T. ) ;
#3463 = PERSON_AND_ORGANIZATION ( #15518, #2538 ) ;
#3464 = CARTESIAN_POINT ( 'NONE',  ( 3.827021247335478926E-17, 3.659999999999999698, 0.3125000000000000000 ) ) ;
#3465 = CARTESIAN_POINT ( 'NONE',  ( -0.5116234456863258950, 3.706421428007538488, -2.785118725032278419 ) ) ;
#3466 = VERTEX_POINT ( 'NONE', #8006 ) ;
#3467 = EDGE_CURVE ( 'NONE', #9682, #22114, #2238, .T. ) ;
#3468 = CARTESIAN_POINT ( 'NONE',  ( -0.3119999999999999996, 0.3131944442927114824, -0.1292346314604056745 ) ) ;
#3469 = LINE ( 'NONE', #12764, #17579 ) ;
#3470 = CARTESIAN_POINT ( 'NONE',  ( 0.3860879860166684940, 4.111524471938507119, -2.831872695974971599 ) ) ;
#3471 = CARTESIAN_POINT ( 'NONE',  ( 0.4700000000000001954, 2.740000000000000213, -2.516000000000000014 ) ) ;
#3472 = DIRECTION ( 'NONE',  ( -0.000000000000000000, -1.000000000000000000, -0.000000000000000000 ) ) ;
#3473 = VERTEX_POINT ( 'NONE', #332 ) ;
#3474 = CARTESIAN_POINT ( 'NONE',  ( -0.1116596296178199582, 0.1758928570453147100, -0.3436530038418508792 ) ) ;
#3475 = CIRCLE ( 'NONE', #5426, 0.2109499999999995268 ) ;
#3476 = EDGE_LOOP ( 'NONE', ( #11159, #7890, #23737, #10078 ) ) ;
#3477 = CARTESIAN_POINT ( 'NONE',  ( 0.2843522314373275739, 5.089490977768033275, -0.1277081573576893947 ) ) ;
#3478 = CARTESIAN_POINT ( 'NONE',  ( -0.2764156081756484196, 0.1144950937579609918, 0.2515277777777809587 ) ) ;
#3479 = CARTESIAN_POINT ( 'NONE',  ( 0.1167790944451422702, 4.113277777853642903, -0.2819296736111110424 ) ) ;
#3480 = CARTESIAN_POINT ( 'NONE',  ( 0.2819296736111110979, 5.158416666742532186, -3.452642723725051716E-17 ) ) ;
#3481 = FACE_OUTER_BOUND ( 'NONE', #43, .T. ) ;
#3482 = CARTESIAN_POINT ( 'NONE',  ( -0.3120000000000000551, 0.3756944442927115380, 0.1292346314604056190 ) ) ;
#3483 = CARTESIAN_POINT ( 'NONE',  ( -0.3119999999999999996, 4.158416666666665762, -0.1292346314604056468 ) ) ;
#3484 = CARTESIAN_POINT ( 'NONE',  ( 0.1292346314604056190, 4.929250000151730760, -0.3119999999999999996 ) ) ;
#3485 = EDGE_CURVE ( 'NONE', #18897, #23410, #14606, .T. ) ;
#3486 = CARTESIAN_POINT ( 'NONE',  ( -0.2819296736111110979, 5.085500000075866112, -0.1167790944451422980 ) ) ;
#3487 = CARTESIAN_POINT ( 'NONE',  ( 1.957333333333323822, 3.718666666666667009, -1.537333333333325669 ) ) ;
#3488 = CARTESIAN_POINT ( 'NONE',  ( -0.1831105892130123203, 0.05713127989799830081, 0.2461514306801097784 ) ) ;
#3489 = VECTOR ( 'NONE', #398, 39.37007874015748143 ) ;
#3490 = ORIENTED_EDGE ( 'NONE', *, *, #7206, .F. ) ;
#3491 = CARTESIAN_POINT ( 'NONE',  ( 0.3155070326520292290, -0.1306872919485616569, 0.2011805555555585268 ) ) ;
#3492 = CARTESIAN_POINT ( 'NONE',  ( 0.2819296736111110979, 5.047305555631421470, -3.452642723725051716E-17 ) ) ;
#3493 = ORIENTED_EDGE ( 'NONE', *, *, #2481, .F. ) ;
#3494 = DIRECTION ( 'NONE',  ( -1.000000000000000000, 0.000000000000000000, 6.148297094540788948E-16 ) ) ;
#3495 = PRODUCT ( 'Aloris-BXA-Center-Shaft', 'Aloris-BXA-Center-Shaft', '', ( #8073 ) ) ;
#3496 = DIRECTION ( 'NONE',  ( 0.8660254037844455910, -0.000000000000000000, -0.4999999999999880096 ) ) ;
#3497 = EDGE_CURVE ( 'NONE', #10744, #3821, #15101, .T. ) ;
#3498 = EDGE_CURVE ( 'NONE', #20299, #20305, #6057, .T. ) ;
#3499 = CARTESIAN_POINT ( 'NONE',  ( -0.2819296736111110979, 0.2437499999241333759, -3.452642723725051716E-17 ) ) ;
#3500 = CARTESIAN_POINT ( 'NONE',  ( 0.1144950937579611444, 0.2764156081756483641, 0.1890277777777804036 ) ) ;
#3501 = CARTESIAN_POINT ( 'NONE',  ( 0.7847114317029997288, 0.000000000000000000, -0.6249999999999962252 ) ) ;
#3502 = CARTESIAN_POINT ( 'NONE',  ( -0.4796768793270155817, -0.08622052910184242747, 0.07157886890657255696 ) ) ;
#3503 = VERTEX_POINT ( 'NONE', #19108 ) ;
#3504 = CARTESIAN_POINT ( 'NONE',  ( -0.2819296736111110979, 4.963972222298087544, 0.000000000000000000 ) ) ;
#3505 = CARTESIAN_POINT ( 'NONE',  ( 1.222470958122163998, 0.000000000000000000, -0.6167782587447089293 ) ) ;
#3506 = VECTOR ( 'NONE', #13354, 39.37007874015748854 ) ;
#3507 = CARTESIAN_POINT ( 'NONE',  ( 0.1891708636127259202, 2.539511724522405989E-17, 0.3078630284654709781 ) ) ;
#3508 = CARTESIAN_POINT ( 'NONE',  ( 0.2597743206613019606, 0.06249999999999967387, 0.1775648204224116178 ) ) ;
#3509 = CARTESIAN_POINT ( 'NONE',  ( 0.3119999999999999996, 4.745222222222221120, -3.820898013339742174E-17 ) ) ;
#3510 = AXIS2_PLACEMENT_3D ( 'NONE', #14109, #12180, #17409 ) ;
#3511 = CARTESIAN_POINT ( 'NONE',  ( 0.1167790944451422702, 4.002166666742532186, -0.2819296736111110979 ) ) ;
#3512 = LINE ( 'NONE', #9118, #4637 ) ;
#3513 = ADVANCED_FACE ( 'NONE', ( #22881 ), #11583, .T. ) ;
#3514 = CARTESIAN_POINT ( 'NONE',  ( 0.2824272245982780150, 4.025992211338290439, 0.1357506634668411982 ) ) ;
#3515 = CARTESIAN_POINT ( 'NONE',  ( -0.006494592122000062383, 0.5491884613158956041, 0.04193801346286451376 ) ) ;
#3516 = ORIENTED_EDGE ( 'NONE', *, *, #10077, .F. ) ;
#3517 = CARTESIAN_POINT ( 'NONE',  ( 3.061616997868382402E-17, 6.000000000000000888, 0.2499999999999999722 ) ) ;
#3518 = EDGE_LOOP ( 'NONE', ( #11149, #9075, #21033, #2947 ) ) ;
#3519 = CARTESIAN_POINT ( 'NONE',  ( 0.2819296736111110979, 4.377166666742532186, 0.1167790944451422425 ) ) ;
#3520 = CARTESIAN_POINT ( 'NONE',  ( -0.3076502150634595201, 4.111722031579642334, -0.05522520306492269965 ) ) ;
#3521 = DIRECTION ( 'NONE',  ( 0.5000000000000007772, 0.000000000000000000, 0.8660254037844382635 ) ) ;
#3522 =( BOUNDED_CURVE ( )  B_SPLINE_CURVE ( 2, ( #21676, #4608, #6553, #6676, #11953, #15711, #944, #8374, #11823 ),
 .UNSPECIFIED., .F., .F. ) 
 B_SPLINE_CURVE_WITH_KNOTS ( ( 3, 2, 2, 2, 3 ),
 ( 0.03786521205662927991, 0.04166666666666673374, 0.05208333333333335646, 0.06249999999999997224, 0.07291666666666669905 ),
 .UNSPECIFIED. ) 
 CURVE ( )  GEOMETRIC_REPRESENTATION_ITEM ( )  RATIONAL_B_SPLINE_CURVE ( ( 0.9647168388458124966, 0.9722206238028953118, 1.000000000000000000, 0.9238795325112867385, 1.000000000000000000, 0.9238795325112867385, 1.000000000000000000, 0.9238795325112870716, 0.9999999999999996669 ) ) 
 REPRESENTATION_ITEM ( '' )  );
#3523 = CIRCLE ( 'NONE', #20648, 1.015181661097394050 ) ;
#3524 = CARTESIAN_POINT ( 'NONE',  ( -0.2764156081756484196, -0.1144950937579609362, 0.1473611111111134686 ) ) ;
#3525 = CARTESIAN_POINT ( 'NONE',  ( -0.3038794998734477004, 3.948928095230931135, 0.08166525255517291526 ) ) ;
#3526 = DIRECTION ( 'NONE',  ( 0.000000000000000000, 1.000000000000000000, 0.000000000000000000 ) ) ;
#3527 = CARTESIAN_POINT ( 'NONE',  ( -0.1954553509668046918, -0.1954553509668046640, 0.3800000000000041678 ) ) ;
#3528 = CARTESIAN_POINT ( 'NONE',  ( 0.3613381517857143232, 0.2973214284738861513, 0.000000000000000000 ) ) ;
#3529 = CARTESIAN_POINT ( 'NONE',  ( 0.2819296736111110979, 0.2020833332574666907, 0.000000000000000000 ) ) ;
#3530 = CARTESIAN_POINT ( 'NONE',  ( 0.4687500000000002776, -0.2570931668155774230, 0.04874733047934001057 ) ) ;
#3531 = CARTESIAN_POINT ( 'NONE',  ( 0.2206173157302028232, 0.5805555555555552694, -0.2206173157302028232 ) ) ;
#3532 = CARTESIAN_POINT ( 'NONE',  ( -0.1613775760850800489, 0.2284702193767794987, -0.7324461116423818252 ) ) ;
#3533 = CARTESIAN_POINT ( 'NONE',  ( 0.2764156081756483641, 0.1144950937579610056, -0.04013888888888804407 ) ) ;
#3534 = EDGE_LOOP ( 'NONE', ( #13556, #12311, #8856, #16838 ) ) ;
#3535 = FACE_OUTER_BOUND ( 'NONE', #9691, .T. ) ;
#3536 = CARTESIAN_POINT ( 'NONE',  ( 0.000000000000000000, 5.501232050807569607, 0.000000000000000000 ) ) ;
#3537 = CARTESIAN_POINT ( 'NONE',  ( 0.1292346314604057023, 0.06319444444444410891, 0.3119999999999998885 ) ) ;
#3538 = CARTESIAN_POINT ( 'NONE',  ( 0.1167790944451424368, 3.773000000075866112, 0.2819296736111110424 ) ) ;
#3539 = CARTESIAN_POINT ( 'NONE',  ( 0.2233192592356399164, 0.2866071427596003640, 0.3073725909049500604 ) ) ;
#3540 = CARTESIAN_POINT ( 'NONE',  ( 0.2819296736111110424, 4.398000000075866112, -0.1167790944451423396 ) ) ;
#3541 = DIRECTION ( 'NONE',  ( 0.5000000000000003331, -0.8660254037844383745, -9.106159978880865562E-16 ) ) ;
#3542 = LINE ( 'NONE', #1714, #10249 ) ;
#3543 = VECTOR ( 'NONE', #14254, 39.37007874015748854 ) ;
#3544 = ORIENTED_EDGE ( 'NONE', *, *, #5352, .T. ) ;
#3545 = CARTESIAN_POINT ( 'NONE',  ( 0.09743210712940192364, 4.374395042175329706, -0.2968164557725501140 ) ) ;
#3546 = CARTESIAN_POINT ( 'NONE',  ( 0.1993543840281267465, 4.873694444520309865, 0.1993543840281266633 ) ) ;
#3547 = CARTESIAN_POINT ( 'NONE',  ( 0.3100836462667937998, 4.197804898758246139, -0.04106420197143005602 ) ) ;
#3548 = CARTESIAN_POINT ( 'NONE',  ( 6.614309848781084774E-13, 0.03242967361111062652, 0.2819296736111109869 ) ) ;
#3549 = CARTESIAN_POINT ( 'NONE',  ( -9.626299801968715084E-16, 0.2035714285714284866, -0.4000000000000000222 ) ) ;
#3550 = CARTESIAN_POINT ( 'NONE',  ( -1.726321361862525858E-17, 4.672305555631421470, -0.2819296736111110979 ) ) ;
#3551 = DATE_TIME_ROLE ( 'classification_date' ) ;
#3552 = CARTESIAN_POINT ( 'NONE',  ( -0.4687500000000004441, 0.2630309001378779987, 0.05971062996526180916 ) ) ;
#3553 = DIRECTION ( 'NONE',  ( 0.000000000000000000, 0.000000000000000000, -1.000000000000000000 ) ) ;
#3554 = CARTESIAN_POINT ( 'NONE',  ( 0.000000000000000000, 0.4199999999999998734, 0.000000000000000000 ) ) ;
#3555 = EDGE_LOOP ( 'NONE', ( #22008, #767, #13904, #22904, #17198, #11031 ) ) ;
#3556 = ORIENTED_EDGE ( 'NONE', *, *, #7501, .T. ) ;
#3557 = CARTESIAN_POINT ( 'NONE',  ( 0.1167790944451423535, 0.1499999999241333759, 0.2819296736111110424 ) ) ;
#3558 = CARTESIAN_POINT ( 'NONE',  ( 0.000000000000000000, 0.01999999999999951469, 0.000000000000000000 ) ) ;
#3559 = CARTESIAN_POINT ( 'NONE',  ( -0.5116234456863466562, 1.808198851485059988, 2.549370209580444691 ) ) ;
#3560 = CARTESIAN_POINT ( 'NONE',  ( 0.4000000000000000222, -0.1000000000000000056, 0.000000000000000000 ) ) ;
#3561 = CARTESIAN_POINT ( 'NONE',  ( -0.3155070326520293400, 0.1306872919485614903, 0.003263888888889874412 ) ) ;
#3562 = CARTESIAN_POINT ( 'NONE',  ( 0.000000000000000000, 0.000000000000000000, 1.326383476483184332 ) ) ;
#3563 = CARTESIAN_POINT ( 'NONE',  ( -0.04794410370418378947, 3.878501262280343198, -0.3084350945838093550 ) ) ;
#3564 = CARTESIAN_POINT ( 'NONE',  ( -0.1167790944451422702, -0.002777777853644409437, -0.2819296736111110424 ) ) ;
#3565 = CARTESIAN_POINT ( 'NONE',  ( -0.1993543840281266355, 4.484805555631421470, 0.1993543840281267465 ) ) ;
#3566 = CARTESIAN_POINT ( 'NONE',  ( 0.1236067977499789028, 0.09107142837634377153, 0.3804226065180614791 ) ) ;
#3567 = CARTESIAN_POINT ( 'NONE',  ( 0.0009234384475589447160, 4.543807118310973614, -0.3119988299807083254 ) ) ;
#3568 = CARTESIAN_POINT ( 'NONE',  ( -0.1993543840281266910, 5.137583333409199149, -0.1993543840281266910 ) ) ;
#3569 = ADVANCED_FACE ( 'NONE', ( #6176 ), #13871, .T. ) ;
#3570 = CARTESIAN_POINT ( 'NONE',  ( -0.1167790944451423535, 4.418833333409199149, 0.2819296736111110979 ) ) ;
#3571 = CARTESIAN_POINT ( 'NONE',  ( 0.2701949539277979651, 3.747486037583882101, 0.1592585331144268646 ) ) ;
#3572 = FACE_OUTER_BOUND ( 'NONE', #18434, .T. ) ;
#3573 = CARTESIAN_POINT ( 'NONE',  ( -0.3853527072884239679, 0.3187823880793517195, 0.07808165802386347887 ) ) ;
#3574 = CARTESIAN_POINT ( 'NONE',  ( -0.1292346314604057023, 4.234805555707287894, 0.3119999999999998885 ) ) ;
#3575 = CARTESIAN_POINT ( 'NONE',  ( -0.1993543840281266910, 4.470916666742532186, -0.1993543840281266910 ) ) ;
#3576 = CARTESIAN_POINT ( 'NONE',  ( 0.1993543840281267465, 3.929250000075865668, 0.1993543840281266633 ) ) ;
#3577 = ORIENTED_EDGE ( 'NONE', *, *, #5971, .F. ) ;
#3578 = ORIENTED_EDGE ( 'NONE', *, *, #10217, .F. ) ;
#3579 = EDGE_LOOP ( 'NONE', ( #1592, #5114, #11152, #15673 ) ) ;
#3580 = DATE_TIME_ROLE ( 'classification_date' ) ;
#3581 = CARTESIAN_POINT ( 'NONE',  ( -0.1292346314604056745, 4.262583333333332725, -0.3119999999999999996 ) ) ;
#3582 = CARTESIAN_POINT ( 'NONE',  ( 0.3119999999999999996, 4.245222222222222008, -3.820898013339742174E-17 ) ) ;
#3583 = CARTESIAN_POINT ( 'NONE',  ( -0.1166234456863465552, 3.066692553488282957, 2.711183489075826181 ) ) ;
#3584 = VERTEX_POINT ( 'NONE', #10097 ) ;
#3585 = CARTESIAN_POINT ( 'NONE',  ( 0.1292346314604056745, 0.2993055554038226429, -0.3119999999999999996 ) ) ;
#3586 = LINE ( 'NONE', #3953, #10138 ) ;
#3587 = CARTESIAN_POINT ( 'NONE',  ( -0.1096552380901288787, 3.735110229336745746, 0.2921016150509060383 ) ) ;
#3588 = DIRECTION ( 'NONE',  ( 0.000000000000000000, 0.000000000000000000, 1.000000000000000000 ) ) ;
#3589 = CARTESIAN_POINT ( 'NONE',  ( 0.000000000000000000, 5.384999999999999787, -0.3119999999999999996 ) ) ;
#3590 = APPROVAL ( #8398, 'UNSPECIFIED' ) ;
#3591 = ORIENTED_EDGE ( 'NONE', *, *, #11260, .F. ) ;
#3592 = CARTESIAN_POINT ( 'NONE',  ( 2.326421213736078119E-17, 0.2437499999024575204, -0.3799334167787516980 ) ) ;
#3593 = ORIENTED_EDGE ( 'NONE', *, *, #20932, .T. ) ;
#3594 = LINE ( 'NONE', #20068, #19681 ) ;
#3595 = CARTESIAN_POINT ( 'NONE',  ( 0.2764156081756483641, 0.1144950937579610056, 0.3418055555555594704 ) ) ;
#3596 = CARTESIAN_POINT ( 'NONE',  ( 0.1993543840281267465, 4.318138888964754507, 0.1993543840281266633 ) ) ;
#3597 = CARTESIAN_POINT ( 'NONE',  ( 5.178964085587577574E-17, 5.144527777853643791, 0.2819296736111110979 ) ) ;
#3598 = CARTESIAN_POINT ( 'NONE',  ( 2.423612122230044959E-16, -0.5289902422706636020, 0.3941886329748525153 ) ) ;
#3599 = CARTESIAN_POINT ( 'NONE',  ( -0.3036941569096411331, 4.222036648323082453, -0.08231831230607603023 ) ) ;
#3600 = CARTESIAN_POINT ( 'NONE',  ( -0.2206173157302027676, 3.946611111111110404, 0.2206173157302028787 ) ) ;
#3601 = CARTESIAN_POINT ( 'NONE',  ( -0.3119999999999998885, 5.005638889040620931, 0.1292346314604058410 ) ) ;
#3602 = AXIS2_PLACEMENT_3D ( 'NONE', #8745, #21683, #1076 ) ;
#3603 = CARTESIAN_POINT ( 'NONE',  ( -0.1167790944451423119, 5.134111111186977716, -0.2819296736111110979 ) ) ;
#3604 = CARTESIAN_POINT ( 'NONE',  ( 0.000000000000000000, 3.700000000000000622, 0.000000000000000000 ) ) ;
#3605 = ORIENTED_EDGE ( 'NONE', *, *, #4937, .T. ) ;
#3606 = CARTESIAN_POINT ( 'NONE',  ( 0.09006919403515362132, 0.04138265269501665428, -0.2775327652233305353 ) ) ;
#3607 = ORIENTED_EDGE ( 'NONE', *, *, #10375, .F. ) ;
#3608 = ADVANCED_FACE ( 'NONE', ( #8121 ), #6779, .F. ) ;
#3609 = CARTESIAN_POINT ( 'NONE',  ( 0.2230971623002954429, 0.2230971623002953319, 0.2671527777777812362 ) ) ;
#3610 = CARTESIAN_POINT ( 'NONE',  ( -1.726321361862525858E-17, 5.116750000075865223, -0.2819296736111110979 ) ) ;
#3611 = ORIENTED_EDGE ( 'NONE', *, *, #22582, .T. ) ;
#3612 = CONICAL_SURFACE ( 'NONE', #13761, 0.2109499999999998043, 1.029744258676653645 ) ;
#3613 = CARTESIAN_POINT ( 'NONE',  ( 0.1904260988303481950, -0.4204977338396739817, 0.4343746145485237187 ) ) ;
#3614 = ADVANCED_FACE ( 'NONE', ( #17518 ), #8240, .F. ) ;
#3615 = CARTESIAN_POINT ( 'NONE',  ( 1.585131139260598010, 2.978485840173427324, -2.498788568296995916 ) ) ;
#3616 = VERTEX_POINT ( 'NONE', #19581 ) ;
#3617 = CARTESIAN_POINT ( 'NONE',  ( -0.1167790944451424506, 0.3097222221463555303, 0.2819296736111110424 ) ) ;
#3618 = CARTESIAN_POINT ( 'NONE',  ( 0.1954553509668046640, -0.1954553509668047195, 0.2827777777777811807 ) ) ;
#3619 = CARTESIAN_POINT ( 'NONE',  ( -1.726321361862525858E-17, 5.019527777853643791, -0.2819296736111110979 ) ) ;
#3620 = CARTESIAN_POINT ( 'NONE',  ( -0.4800173708727313859, -0.1715353579592617805, 0.06110628606926749029 ) ) ;
#3621 = ORIENTED_EDGE ( 'NONE', *, *, #10624, .T. ) ;
#3622 = CARTESIAN_POINT ( 'NONE',  ( -0.1993543840281266355, 4.915361111186976828, 0.1993543840281267465 ) ) ;
#3623 = PLANE ( 'NONE',  #1336 ) ;
#3624 = CARTESIAN_POINT ( 'NONE',  ( -0.3119999999999999996, 5.050777777777776478, 0.000000000000000000 ) ) ;
#3625 = CARTESIAN_POINT ( 'NONE',  ( 0.000000000000000000, 3.669999999999999929, 0.000000000000000000 ) ) ;
#3626 = CARTESIAN_POINT ( 'NONE',  ( 0.1292346314604056745, 0.5840277777777773682, -0.3119999999999999996 ) ) ;
#3627 = CARTESIAN_POINT ( 'NONE',  ( 0.2206173157302028787, 4.404944444444443441, 0.2206173157302027954 ) ) ;
#3628 = CARTESIAN_POINT ( 'NONE',  ( -0.1167790944451423535, 4.029944444520309865, 0.2819296736111110979 ) ) ;
#3629 = CARTESIAN_POINT ( 'NONE',  ( 0.000000000000000000, 2.689999999999999947, -2.165185842870423816 ) ) ;
#3630 = CARTESIAN_POINT ( 'NONE',  ( 0.1383926702065426950, 4.020153189153055528, 0.2803734965809290824 ) ) ;
#3631 = CARTESIAN_POINT ( 'NONE',  ( 0.006583943204587710575, 0.5374646359837784715, 0.05971082423030439623 ) ) ;
#3632 = ORIENTED_EDGE ( 'NONE', *, *, #17864, .T. ) ;
#3633 = ORIENTED_EDGE ( 'NONE', *, *, #13120, .F. ) ;
#3634 = CARTESIAN_POINT ( 'NONE',  ( 0.000000000000000000, 0.4202679491924311006, 0.000000000000000000 ) ) ;
#3635 = ORIENTED_EDGE ( 'NONE', *, *, #8017, .F. ) ;
#3636 = AXIS2_PLACEMENT_3D ( 'NONE', #3554, #11005, #18433 ) ;
#3637 = CARTESIAN_POINT ( 'NONE',  ( -0.2592333949642908197, 4.108027434044173809, -0.1776828664482337783 ) ) ;
#3638 = EDGE_CURVE ( 'NONE', #8540, #1241, #21598, .T. ) ;
#3639 = EDGE_CURVE ( 'NONE', #23261, #3437, #1175, .T. ) ;
#3640 = CARTESIAN_POINT ( 'NONE',  ( 0.09694982473845883963, 0.06249891840240667101, 0.2965547697865978938 ) ) ;
#3641 = CARTESIAN_POINT ( 'NONE',  ( 0.1144950937579609085, -0.2764156081756484751, 0.2723611111111144401 ) ) ;
#3642 = CARTESIAN_POINT ( 'NONE',  ( 0.000000000000000000, 6.000000000000000888, 0.000000000000000000 ) ) ;
#3643 = EDGE_CURVE ( 'NONE', #8247, #20864, #10439, .T. ) ;
#3644 = LINE ( 'NONE', #20235, #21852 ) ;
#3645 = CARTESIAN_POINT ( 'NONE',  ( 1.090085390906250263E-17, 0.2597990586171761707, -1.138795812253956763 ) ) ;
#3646 = CARTESIAN_POINT ( 'NONE',  ( 0.2233192592356399164, 0.3580357141881718164, 0.3073725909049500604 ) ) ;
#3647 = CARTESIAN_POINT ( 'NONE',  ( -5.178964085587577574E-17, 0.2993055554796889561, 0.2819296736111110979 ) ) ;
#3648 = DIRECTION ( 'NONE',  ( 0.000000000000000000, 1.000000000000000000, 0.000000000000000000 ) ) ;
#3649 = CARTESIAN_POINT ( 'NONE',  ( -5.731347020009612645E-17, 0.5597222222222218990, 0.3119999999999999996 ) ) ;
#3650 = CARTESIAN_POINT ( 'NONE',  ( 0.8119709581221709049, 0.000000000000000000, -1.327785115251736814 ) ) ;
#3651 = CARTESIAN_POINT ( 'NONE',  ( -0.2764156081756484196, -0.1144950937579609362, -0.01236111111111004406 ) ) ;
#3652 = VECTOR ( 'NONE', #18771, 39.37007874015748143 ) ;
#3653 = EDGE_LOOP ( 'NONE', ( #6556, #19153, #18472, #12719 ) ) ;
#3654 = ORIENTED_EDGE ( 'NONE', *, *, #9559, .F. ) ;
#3655 = CARTESIAN_POINT ( 'NONE',  ( -0.2786000101406610474, 5.109152158301237812, 0.1360994231350151629 ) ) ;
#3656 = CARTESIAN_POINT ( 'NONE',  ( 0.4687499999999811262, 0.04487173304136180679, 0.4280330084738984131 ) ) ;
#3657 = CARTESIAN_POINT ( 'NONE',  ( 0.3119999999999999996, 0.02152777777777744109, -0.1292346314604056468 ) ) ;
#3658 = CARTESIAN_POINT ( 'NONE',  ( -0.1167790944451423257, 3.911888888964754507, -0.2819296736111110424 ) ) ;
#3659 = CARTESIAN_POINT ( 'NONE',  ( -6.979263641208234666E-17, 0.1366071427596004251, 0.3799334167787516425 ) ) ;
#3660 = ORIENTED_EDGE ( 'NONE', *, *, #15494, .T. ) ;
#3661 = CARTESIAN_POINT ( 'NONE',  ( 0.2819296736111110424, 4.509111111186976828, -0.1167790944451423396 ) ) ;
#3662 = CARTESIAN_POINT ( 'NONE',  ( -1.910449006669871087E-17, 4.981333333333332725, -0.3119999999999999996 ) ) ;
#3663 = CARTESIAN_POINT ( 'NONE',  ( 0.000000000000000000, 2.777857142857143913, -2.063737152712815881 ) ) ;
#3664 = ORIENTED_EDGE ( 'NONE', *, *, #7956, .F. ) ;
#3665 = CARTESIAN_POINT ( 'NONE',  ( 5.731347020009612645E-17, 4.675777777777777366, 0.3119999999999999996 ) ) ;
#3666 = CARTESIAN_POINT ( 'NONE',  ( -0.1993543840281266910, 4.901472222298087544, -0.1993543840281266910 ) ) ;
#3667 =( BOUNDED_CURVE ( )  B_SPLINE_CURVE ( 2, ( #18228, #15794, #6522, #21402, #2857, #17743, #1038, #8467, #15908 ),
 .UNSPECIFIED., .F., .F. ) 
 B_SPLINE_CURVE_WITH_KNOTS ( ( 3, 2, 2, 2, 3 ),
 ( 0.7291666666666666297, 0.7395833333333333703, 0.7500000000000000000, 0.7604166666666666297, 0.7708333333333333703 ),
 .UNSPECIFIED. ) 
 CURVE ( )  GEOMETRIC_REPRESENTATION_ITEM ( )  RATIONAL_B_SPLINE_CURVE ( ( 1.000000000000000000, 0.9238795325112867385, 1.000000000000000000, 0.9238795325112867385, 1.000000000000000000, 0.9238795325112867385, 1.000000000000000000, 0.9238795325112867385, 1.000000000000000000 ) ) 
 REPRESENTATION_ITEM ( '' )  );
#3668 = EDGE_CURVE ( 'NONE', #15698, #11818, #15573, .T. ) ;
#3669 = LINE ( 'NONE', #3792, #11079 ) ;
#3670 = VECTOR ( 'NONE', #3942, 39.37007874015748854 ) ;
#3671 = SHAPE_REPRESENTATION_RELATIONSHIP ( 'NONE' , 'NONE' ,  #7952, #12638 ) ;
#3672 = CARTESIAN_POINT ( 'NONE',  ( 0.4000000000000000222, 0.1857142857142856651, 0.000000000000000000 ) ) ;
#3673 = CARTESIAN_POINT ( 'NONE',  ( -0.1993543840281266355, 4.693138888964754507, 0.1993543840281267465 ) ) ;
#3674 = ITEM_DEFINED_TRANSFORMATION ( 'NONE', 'NONE', #16539,  #9127 ) ;
#3675 = DIRECTION ( 'NONE',  ( 0.000000000000000000, 0.000000000000000000, 1.000000000000000000 ) ) ;
#3676 = DIRECTION ( 'NONE',  ( -1.000000000000000000, 0.000000000000000000, -0.000000000000000000 ) ) ;
#3677 = VECTOR ( 'NONE', #20766, 39.37007874015748143 ) ;
#3678 = CARTESIAN_POINT ( 'NONE',  ( -0.2819296736111110424, 0.5180555554796888451, -0.1167790944451423396 ) ) ;
#3679 = ORIENTED_EDGE ( 'NONE', *, *, #6592, .T. ) ;
#3680 = VERTEX_POINT ( 'NONE', #928 ) ;
#3681 = CARTESIAN_POINT ( 'NONE',  ( 0.2819296736111110424, 0.2124999999241334314, 0.1167790944451424923 ) ) ;
#3682 = CARTESIAN_POINT ( 'NONE',  ( -0.3119999999999998885, 4.332027777777777366, 0.1292346314604058410 ) ) ;
#3683 = CARTESIAN_POINT ( 'NONE',  ( -0.2839807072535898147, 5.201861426142459166, 0.01683923060391288168 ) ) ;
#3684 = CARTESIAN_POINT ( 'NONE',  ( -0.2472135954999579444, 0.2821428571428570287, -0.3402603233408159622 ) ) ;
#3685 = CARTESIAN_POINT ( 'NONE',  ( 0.3155070326520292290, 0.1306872919485615736, -0.07312499999999962086 ) ) ;
#3686 = CARTESIAN_POINT ( 'NONE',  ( -0.4570242136016808843, -0.2774028246161672762, 0.04874733047933989261 ) ) ;
#3687 = CARTESIAN_POINT ( 'NONE',  ( -0.2173539347745672701, 3.883923987474912298, -0.2247910917580860646 ) ) ;
#3688 = CARTESIAN_POINT ( 'NONE',  ( -0.2819296736111111534, 0.2333333332574667185, 0.1167790944451422563 ) ) ;
#3689 = CARTESIAN_POINT ( 'NONE',  ( -0.2819296736111110979, 0.007638888813022256218, -3.452642723725051716E-17 ) ) ;
#3690 = CARTESIAN_POINT ( 'NONE',  ( -0.1167790944451423257, 4.411888888964754507, -0.2819296736111110424 ) ) ;
#3691 = CARTESIAN_POINT ( 'NONE',  ( -0.3236067977499790249, 0.005357142662058073795, 0.2351141009169892271 ) ) ;
#3692 = CARTESIAN_POINT ( 'NONE',  ( 0.000000000000000000, 0.000000000000000000, -0.05999999999999999084 ) ) ;
#3693 = AXIS2_PLACEMENT_3D ( 'NONE', #22291, #3884, #2054 ) ;
#3694 = CARTESIAN_POINT ( 'NONE',  ( -0.2819296736111110424, 5.203555555631421470, 0.1167790944451424923 ) ) ;
#3695 = CARTESIAN_POINT ( 'NONE',  ( 5.178964085587577574E-17, 4.422305555631421470, 0.2819296736111110979 ) ) ;
#3696 = CARTESIAN_POINT ( 'NONE',  ( 0.3088587430578357274, 3.750936470065025841, 0.04450246037814264283 ) ) ;
#3697 = DIRECTION ( 'NONE',  ( 1.000000000000000000, 0.000000000000000000, 0.000000000000000000 ) ) ;
#3698 = CARTESIAN_POINT ( 'NONE',  ( 0.3003959655288142017, 3.916143348187413498, 0.09367083608899910707 ) ) ;
#3699 = CARTESIAN_POINT ( 'NONE',  ( 0.3119999999999999996, 4.082027777929511103, 0.1292346314604056190 ) ) ;
#3700 = CARTESIAN_POINT ( 'NONE',  ( -1.726321361862525858E-17, 4.575083333409199149, -0.2819296736111110979 ) ) ;
#3701 = CC_DESIGN_APPROVAL ( #10165, ( #11902 ) ) ;
#3702 = VERTEX_POINT ( 'NONE', #8358 ) ;
#3703 = ORIENTED_EDGE ( 'NONE', *, *, #385, .T. ) ;
#3704 = ADVANCED_FACE ( 'NONE', ( #23227 ), #21658, .T. ) ;
#3705 = APPROVAL_DATE_TIME ( #7367, #14170 ) ;
#3706 = AXIS2_PLACEMENT_3D ( 'NONE', #10467, #6795, #10225 ) ;
#3707 = EDGE_CURVE ( 'NONE', #7602, #22848, #22539, .T. ) ;
#3708 = CARTESIAN_POINT ( 'NONE',  ( 0.000000000000000000, 0.000000000000000000, 1.326383476483184332 ) ) ;
#3709 = DIRECTION ( 'NONE',  ( 0.000000000000000000, 0.000000000000000000, 1.000000000000000000 ) ) ;
#3710 = ORIENTED_EDGE ( 'NONE', *, *, #3497, .T. ) ;
#3711 = CARTESIAN_POINT ( 'NONE',  ( 0.3119999999999999996, 0.4590277776260447973, -0.1292346314604056468 ) ) ;
#3712 = ORIENTED_EDGE ( 'NONE', *, *, #7688, .F. ) ;
#3713 = CYLINDRICAL_SURFACE ( 'NONE', #22592, 0.3119999999999999996 ) ;
#3714 = CARTESIAN_POINT ( 'NONE',  ( -0.2767634618065506480, 3.728737891010954542, 0.1512181958280439387 ) ) ;
#3715 = CARTESIAN_POINT ( 'NONE',  ( -0.3120000000000000551, 0.2715277777777774793, 0.1292346314604056190 ) ) ;
#3716 = LINE ( 'NONE', #13129, #15145 ) ;
#3717 =( BOUNDED_CURVE ( )  B_SPLINE_CURVE ( 2, ( #6409, #12526, #17998, #17507, #1167, #14215, #17629, #2865, #23460 ),
 .UNSPECIFIED., .F., .F. ) 
 B_SPLINE_CURVE_WITH_KNOTS ( ( 3, 2, 2, 2, 3 ),
 ( 0.3125000000000000000, 0.3229166666666666852, 0.3333333333333333148, 0.3437500000000000000, 0.3541666666666666852 ),
 .UNSPECIFIED. ) 
 CURVE ( )  GEOMETRIC_REPRESENTATION_ITEM ( )  RATIONAL_B_SPLINE_CURVE ( ( 1.000000000000000000, 0.9238795325112867385, 1.000000000000000000, 0.9238795325112867385, 1.000000000000000000, 0.9238795325112867385, 1.000000000000000000, 0.9238795325112867385, 1.000000000000000000 ) ) 
 REPRESENTATION_ITEM ( '' )  );
#3718 = ORIENTED_EDGE ( 'NONE', *, *, #6207, .F. ) ;
#3719 = ORIENTED_EDGE ( 'NONE', *, *, #23371, .F. ) ;
#3720 = APPROVAL_PERSON_ORGANIZATION ( #22837, #5523, #6125 ) ;
#3721 = CARTESIAN_POINT ( 'NONE',  ( -0.3613381517857143232, 0.04732142847388616513, -4.425116109941954795E-17 ) ) ;
#3722 = ORIENTED_EDGE ( 'NONE', *, *, #467, .F. ) ;
#3723 = CARTESIAN_POINT ( 'NONE',  ( 0.3110505074677553661, 5.085000275326436281, 0.02324247747823024457 ) ) ;
#3724 = CARTESIAN_POINT ( 'NONE',  ( 0.1144950937579609085, -0.2764156081756484751, 0.2723611111111144401 ) ) ;
#3725 = CARTESIAN_POINT ( 'NONE',  ( 0.1993543840281266633, 4.165361111186975940, -0.1993543840281266910 ) ) ;
#3726 = CARTESIAN_POINT ( 'NONE',  ( -1.726321361862525858E-17, 5.116750000075865223, -0.2819296736111110979 ) ) ;
#3727 = LINE ( 'NONE', #16419, #7894 ) ;
#3728 = CARTESIAN_POINT ( 'NONE',  ( 0.3950000000000000733, 2.978485840173427324, -0.6605837454876625214 ) ) ;
#3729 = CARTESIAN_POINT ( 'NONE',  ( -1.910449006669871087E-17, 3.870222222222221564, -0.3119999999999999996 ) ) ;
#3730 = CARTESIAN_POINT ( 'NONE',  ( -0.1292346314604056745, 4.769527777929509327, -0.3119999999999999996 ) ) ;
#3731 = AXIS2_PLACEMENT_3D ( 'NONE', #15801, #13980, #21408 ) ;
#3732 = CARTESIAN_POINT ( 'NONE',  ( 0.2819296736111111534, 5.113277777853642903, 0.1167790944451422563 ) ) ;
#3733 = CARTESIAN_POINT ( 'NONE',  ( 0.2206173157302027676, 0.3999999999999996336, 0.2206173157302028787 ) ) ;
#3734 = CARTESIAN_POINT ( 'NONE',  ( 2.326421213736078119E-17, 0.2258928570453146711, -0.3799334167787516980 ) ) ;
#3735 = APPROVAL ( #2630, 'UNSPECIFIED' ) ;
#3736 = SECURITY_CLASSIFICATION ( '', '', #14901 ) ;
#3737 = DIRECTION ( 'NONE',  ( 0.8459207832372976910, 0.4883925919151544948, 0.2142211582677918946 ) ) ;
#3738 = ORIENTED_EDGE ( 'NONE', *, *, #7836, .T. ) ;
#3739 = APPROVAL_ROLE ( '' ) ;
#3740 = CARTESIAN_POINT ( 'NONE',  ( -0.2230971623002954152, -0.2230971623002953874, 0.2393750000000033074 ) ) ;
#3741 = CARTESIAN_POINT ( 'NONE',  ( 0.2819296736111110979, 5.158416666742532186, -3.452642723725051716E-17 ) ) ;
#3742 = CLOSED_SHELL ( 'NONE', ( #4111, #9837, #17596, #2860, #19851, #10733, #13501, #22727, #19441, #9629, #12004, #16611, #8942, #23112, #13635, #5190, #10403 ) ) ;
#3743 = DIRECTION ( 'NONE',  ( 1.000000000000000000, 0.000000000000000000, -0.000000000000000000 ) ) ;
#3744 = B_SPLINE_CURVE_WITH_KNOTS ( 'NONE', 3,
 ( #23433, #4672, #10648, #6741, #6865, #16380, #14185, #8687, #1380, #12141, #21619, #19548, #18080, #4912, #14308, #13954, #12374, #16135, #8809, #6619, #10423, #19792, #5027, #17723, #17848, #16258, #23670, #10299, #14070, #3091, #10534, #1139, #8574, #2967, #15892, #23312, #3202, #21497, #16015, #12492, #6989, #21742, #19913, #12254, #14431 ),
 .UNSPECIFIED., .F., .F.,
 ( 4, 2, 2, 2, 2, 1, 1, 1, 2, 2, 1, 2, 2, 2, 2, 2, 1, 2, 2, 2, 2, 2, 2, 2, 4 ),
 ( 0.09617319050982510442, 0.09758660992310271010, 0.09900002933638030189, 0.1018268681629354994, 0.1046537069894907107, 0.1050070618428101121, 0.1051837392694698059, 0.1052720779827996528, 0.1053162473394645832, 0.1053383320177970345, 0.1053604166961294997, 0.1060671264027681776, 0.1074805458160455335, 0.1088939652293229032, 0.1103073846426002591, 0.1117208040558776150, 0.1118974814825372810, 0.1119858201958671140, 0.1120741589091969470, 0.1124275137625162929, 0.1131342234691549709, 0.1145476428824323267, 0.1159610622957096826, 0.1173744817089870524, 0.1187879011222644082 ),
 .UNSPECIFIED. ) ;
#3745 = CARTESIAN_POINT ( 'NONE',  ( 0.2923287055106771337, 0.4151785713310289228, 0.2123892367102621359 ) ) ;
#3746 = CARTESIAN_POINT ( 'NONE',  ( 1.726321361862525858E-17, 0.1743055554796889284, -0.2819296736111110979 ) ) ;
#3747 = CARTESIAN_POINT ( 'NONE',  ( -0.2764156081756484196, 0.1144950937579609918, 0.1473611111111134686 ) ) ;
#3748 = CARTESIAN_POINT ( 'NONE',  ( -0.2819296736111110424, 4.925777777853643791, 0.1167790944451424923 ) ) ;
#3749 = CARTESIAN_POINT ( 'NONE',  ( 0.1661407850955833043, 4.483412766610799238, -0.2646232894162082183 ) ) ;
#3750 = CARTESIAN_POINT ( 'NONE',  ( -1.726321361862525858E-17, 4.950083333409199149, -0.2819296736111110979 ) ) ;
#3751 = DIRECTION ( 'NONE',  ( 0.4999999999999916178, 0.000000000000000000, -0.8660254037844433705 ) ) ;
#3752 = EDGE_CURVE ( 'NONE', #10167, #13618, #14222, .T. ) ;
#3753 = DIRECTION ( 'NONE',  ( 0.8660254037844431485, 0.000000000000000000, 0.4999999999999918954 ) ) ;
#3754 = LOCAL_TIME ( 21, 9, 13.00000000000000000, #22808 ) ;
#3755 = CARTESIAN_POINT ( 'NONE',  ( 0.2206173157302027954, 4.085499999999999687, -0.2206173157302028232 ) ) ;
#3756 = CARTESIAN_POINT ( 'NONE',  ( 1.829696540937382654, 2.476534978792082065, -1.949930308767543030 ) ) ;
#3757 = CARTESIAN_POINT ( 'NONE',  ( -0.2206173157302028232, 4.432722222222222008, -0.2206173157302028232 ) ) ;
#3758 = CARTESIAN_POINT ( 'NONE',  ( 0.2819296736111111534, 3.932722222298087988, 0.1167790944451422563 ) ) ;
#3759 = CARTESIAN_POINT ( 'NONE',  ( 0.2510000000000000009, 0.4997679491924311157, 0.000000000000000000 ) ) ;
#3760 = CARTESIAN_POINT ( 'NONE',  ( 0.04088167920887831458, 4.017269169224574554, 0.3120000053084774350 ) ) ;
#3761 = DIRECTION ( 'NONE',  ( 0.000000000000000000, 0.000000000000000000, -1.000000000000000000 ) ) ;
#3762 = ORIENTED_EDGE ( 'NONE', *, *, #4520, .F. ) ;
#3763 = VECTOR ( 'NONE', #14700, 39.37007874015748143 ) ;
#3764 = CARTESIAN_POINT ( 'NONE',  ( 0.000000000000000000, 3.700000000000000622, 0.000000000000000000 ) ) ;
#3765 = ORIENTED_EDGE ( 'NONE', *, *, #18070, .T. ) ;
#3766 =( BOUNDED_CURVE ( )  B_SPLINE_CURVE ( 2, ( #14387, #15853, #14145, #21461, #19751, #3047, #3886, #103, #5592 ),
 .UNSPECIFIED., .F., .F. ) 
 B_SPLINE_CURVE_WITH_KNOTS ( ( 3, 2, 2, 2, 3 ),
 ( 0.6041666666666666297, 0.6145833333333333703, 0.6250000000000000000, 0.6354166666666666297, 0.6458333333333333703 ),
 .UNSPECIFIED. ) 
 CURVE ( )  GEOMETRIC_REPRESENTATION_ITEM ( )  RATIONAL_B_SPLINE_CURVE ( ( 1.000000000000000000, 0.9238795325112867385, 1.000000000000000000, 0.9238795325112867385, 1.000000000000000000, 0.9238795325112867385, 1.000000000000000000, 0.9238795325112867385, 1.000000000000000000 ) ) 
 REPRESENTATION_ITEM ( '' )  );
#3767 = CC_DESIGN_DATE_AND_TIME_ASSIGNMENT ( #12998, #16276, ( #2554 ) ) ;
#3768 = CARTESIAN_POINT ( 'NONE',  ( -0.2356117178940455303, 4.106961824400430672, -0.2079910394304901600 ) ) ;
#3769 = CARTESIAN_POINT ( 'NONE',  ( -3.385114897866767815E-17, -0.2764156081756484196, 0.2688888888888921747 ) ) ;
#3770 = DIRECTION ( 'NONE',  ( 0.000000000000000000, 0.000000000000000000, -1.000000000000000000 ) ) ;
#3771 = CARTESIAN_POINT ( 'NONE',  ( 0.000000000000000000, 5.579732050807569621, 0.000000000000000000 ) ) ;
#3772 = CARTESIAN_POINT ( 'NONE',  ( 0.3613381517857143232, 0.3651785713310288783, 0.1174058825155742114 ) ) ;
#3773 = AXIS2_PLACEMENT_3D ( 'NONE', #22577, #498, #15386 ) ;
#3774 = CARTESIAN_POINT ( 'NONE',  ( 0.2819296736111110979, 0.2576388888130222155, 0.000000000000000000 ) ) ;
#3775 = CARTESIAN_POINT ( 'NONE',  ( -0.2977100099089716734, 3.575000000000000622, -0.09499999999999993172 ) ) ;
#3776 = CARTESIAN_POINT ( 'NONE',  ( -5.308788303787306404E-17, 0.03949697488198145034, 0.2889969748819818385 ) ) ;
#3777 = CARTESIAN_POINT ( 'NONE',  ( -0.3124999999999989453, -0.1294417382415932460, 0.06402777777777933499 ) ) ;
#3778 = CARTESIAN_POINT ( 'NONE',  ( 0.1954553509668046640, -0.1954553509668047195, 0.005000000000001192726 ) ) ;
#3779 = CARTESIAN_POINT ( 'NONE',  ( 0.03174294256098306871, 0.01825705743901666692, -0.6191099248581333203 ) ) ;
#3780 = CARTESIAN_POINT ( 'NONE',  ( 0.1292346314604007063, 4.366749999999999687, -0.3120000000000049400 ) ) ;
#3781 = CARTESIAN_POINT ( 'NONE',  ( -0.2819296736111110979, 0.5631944443685777957, -3.452642723725051716E-17 ) ) ;
#3782 = CARTESIAN_POINT ( 'NONE',  ( 0.2206173157302028787, 5.071611111111109516, 0.2206173157302027954 ) ) ;
#3783 = CARTESIAN_POINT ( 'NONE',  ( 0.3613381517857143232, 0.2973214284738861513, 0.000000000000000000 ) ) ;
#3784 = EDGE_CURVE ( 'NONE', #16705, #4879, #10333, .T. ) ;
#3785 = CARTESIAN_POINT ( 'NONE',  ( -0.2819296736111110979, 4.311194444520309865, 0.000000000000000000 ) ) ;
#3786 = CARTESIAN_POINT ( 'NONE',  ( 0.3119999999999999996, 4.967444444444443441, -3.820898013339742174E-17 ) ) ;
#3787 = CARTESIAN_POINT ( 'NONE',  ( 0.3208197908154664102, -2.427762526784287634E-18, -0.1679480024125937221 ) ) ;
#3788 = ORIENTED_EDGE ( 'NONE', *, *, #3849, .F. ) ;
#3789 = CARTESIAN_POINT ( 'NONE',  ( 0.2677646337359513851, 4.358477931348908818, 0.1602620551619879097 ) ) ;
#3790 = CARTESIAN_POINT ( 'NONE',  ( -0.2819296736111110424, 5.016055555631420582, -0.1167790944451423119 ) ) ;
#3791 = ADVANCED_FACE ( 'NONE', ( #23469 ), #1054, .T. ) ;
#3792 = CARTESIAN_POINT ( 'NONE',  ( 3.820898013339742174E-17, 0.06249999999999967387, -0.3119999999999999996 ) ) ;
#3793 = AXIS2_PLACEMENT_3D ( 'NONE', #10115, #6436, #17540 ) ;
#3794 = CARTESIAN_POINT ( 'NONE',  ( 2.285102959650015197, 2.697839921951305175, -2.464255729834791797 ) ) ;
#3795 = DIRECTION ( 'NONE',  ( -0.000000000000000000, -1.000000000000000000, -0.000000000000000000 ) ) ;
#3796 = B_SPLINE_CURVE_WITH_KNOTS ( 'NONE', 3,
 ( #5158, #10432, #14195, #23561, #19925, #10305 ),
 .UNSPECIFIED., .F., .F.,
 ( 4, 2, 4 ),
 ( 0.3494352842492303157, 0.4117316744839973897, 0.4740280647187645191 ),
 .UNSPECIFIED. ) ;
#3797 = CARTESIAN_POINT ( 'NONE',  ( 0.2819296736111110979, 4.773000000075865223, -0.1167790944451423396 ) ) ;
#3798 = CALENDAR_DATE ( 2026, 7, 10 ) ;
#3799 = LINE ( 'NONE', #1970, #15615 ) ;
#3800 = DIRECTION ( 'NONE',  ( -0.000000000000000000, -1.000000000000000000, -0.000000000000000000 ) ) ;
#3801 = CARTESIAN_POINT ( 'NONE',  ( -0.2819296736111110979, 0.4659722221463555303, -3.452642723725051716E-17 ) ) ;
#3802 = EDGE_LOOP ( 'NONE', ( #2222, #17313, #22434, #23234 ) ) ;
#3803 = ORIENTED_EDGE ( 'NONE', *, *, #8915, .T. ) ;
#3804 = CARTESIAN_POINT ( 'NONE',  ( 0.1167790944451423257, 0.1708333332574666907, -0.2819296736111110424 ) ) ;
#3805 = CARTESIAN_POINT ( 'NONE',  ( 0.6398935782932173577, 7.836436224517350621E-17, -0.1019043464467004889 ) ) ;
#3806 = CARTESIAN_POINT ( 'NONE',  ( -0.1294417382415922746, -0.3125000000000000000, 0.1820833333333357340 ) ) ;
#3807 = CARTESIAN_POINT ( 'NONE',  ( -7.726019084026502927E-17, 0.3107142857142856096, 0.4205848896953069405 ) ) ;
#3808 = CARTESIAN_POINT ( 'NONE',  ( -0.3155070326520293400, -0.1306872919485614626, -0.1009027777777776053 ) ) ;
#3809 = CARTESIAN_POINT ( 'NONE',  ( 0.4687500000000002776, -0.2386081413226768533, 0.3840704193421530244 ) ) ;
#3810 = CARTESIAN_POINT ( 'NONE',  ( 0.3120000000000000551, 5.019527777777777366, 0.1292346314604056190 ) ) ;
#3811 = CARTESIAN_POINT ( 'NONE',  ( 0.2819296736111110424, 0.1986111110352444531, 0.1167790944451424923 ) ) ;
#3812 = CARTESIAN_POINT ( 'NONE',  ( 1.095241930731965629, 2.405295409249399441, -1.047581479122380754 ) ) ;
#3813 = EDGE_CURVE ( 'NONE', #4009, #1058, #2530, .T. ) ;
#3814 = ADVANCED_FACE ( 'NONE', ( #4467, #18123 ), #7029, .T. ) ;
#3815 = CARTESIAN_POINT ( 'NONE',  ( 0.2819296736111110979, 4.279944444520310753, 0.1167790944451422425 ) ) ;
#3816 = VECTOR ( 'NONE', #13139, 39.37007874015748143 ) ;
#3817 = CARTESIAN_POINT ( 'NONE',  ( 2.575339694675500462E-17, 0.1232142855192008835, -0.4205848896953069405 ) ) ;
#3818 = CARTESIAN_POINT ( 'NONE',  ( -0.2819296736111110424, 5.085500000075866112, -0.1167790944451423119 ) ) ;
#3819 = CARTESIAN_POINT ( 'NONE',  ( 0.1167790944451424506, 4.536888888964754507, 0.2819296736111110424 ) ) ;
#3820 = DIRECTION ( 'NONE',  ( -0.7071067811865475727, -0.000000000000000000, -0.7071067811865475727 ) ) ;
#3821 = VERTEX_POINT ( 'NONE', #7151 ) ;
#3822 = CARTESIAN_POINT ( 'NONE',  ( -0.4593750000000004219, 0.2760455974562898707, 0.06112444011295372487 ) ) ;
#3823 = CARTESIAN_POINT ( 'NONE',  ( -0.3119999999999999996, 4.054250000151732536, -0.1292346314604056468 ) ) ;
#3824 = EDGE_CURVE ( 'NONE', #10167, #14330, #20073, .T. ) ;
#3825 = CARTESIAN_POINT ( 'NONE',  ( -1.726321361862525858E-17, 3.727861111186976384, -0.2819296736111110979 ) ) ;
#3826 = CARTESIAN_POINT ( 'NONE',  ( 0.004657599350281299740, -0.3068592482405122501, -0.09560169298593859666 ) ) ;
#3827 = ORIENTED_EDGE ( 'NONE', *, *, #18211, .T. ) ;
#3828 = AXIS2_PLACEMENT_3D ( 'NONE', #10600, #5091, #8386 ) ;
#3829 = ORIENTED_EDGE ( 'NONE', *, *, #10998, .F. ) ;
#3830 = APPLICATION_PROTOCOL_DEFINITION ( 'international standard', 'config_control_design', 1994, #7951 ) ;
#3831 = LINE ( 'NONE', #1876, #3763 ) ;
#3832 = CARTESIAN_POINT ( 'NONE',  ( 0.1899274842524382167, -0.4207833852643003136, 0.4343212420608418833 ) ) ;
#3833 = CARTESIAN_POINT ( 'NONE',  ( 2.458533612140684792E-17, 0.1592944763917982509, -1.165725933896874400 ) ) ;
#3834 = ORIENTED_EDGE ( 'NONE', *, *, #23371, .T. ) ;
#3835 = CARTESIAN_POINT ( 'NONE',  ( 0.1292346314604057023, 0.5562499998482671737, 0.3119999999999998885 ) ) ;
#3836 = ORIENTED_EDGE ( 'NONE', *, *, #12285, .F. ) ;
#3837 = CARTESIAN_POINT ( 'NONE',  ( -0.3125000000000000555, 1.913510623667739771E-17, 0.1786111111111139127 ) ) ;
#3838 = CARTESIAN_POINT ( 'NONE',  ( 0.2697513640123151979, 4.756947486709429462, -0.1629237773733702710 ) ) ;
#3839 = CARTESIAN_POINT ( 'NONE',  ( 0.1116596296178199027, -0.02053571438325667992, 0.3436530038418508792 ) ) ;
#3840 = CARTESIAN_POINT ( 'NONE',  ( 1.910449006669871087E-17, 0.4763888888888885287, -0.3119999999999999996 ) ) ;
#3841 = ORIENTED_EDGE ( 'NONE', *, *, #1780, .F. ) ;
#3842 = CARTESIAN_POINT ( 'NONE',  ( 0.2923287055106771337, 0.01874999990245761194, -0.2123892367102620249 ) ) ;
#3843 = DIRECTION ( 'NONE',  ( 0.000000000000000000, -0.9961946980917454342, -0.08715574274765842955 ) ) ;
#3844 = CARTESIAN_POINT ( 'NONE',  ( -0.2206173157302028232, 4.043833333333332725, -0.2206173157302028232 ) ) ;
#3845 = CARTESIAN_POINT ( 'NONE',  ( -0.2819296736111110979, 4.241750000075865223, 0.000000000000000000 ) ) ;
#3846 = CARTESIAN_POINT ( 'NONE',  ( 1.910449006669871087E-17, 0.3027777776260448528, -0.3119999999999999996 ) ) ;
#3847 = CARTESIAN_POINT ( 'NONE',  ( -0.2026594160797258459, 0.4367605021652133379, 0.07441357458167799366 ) ) ;
#3848 = CARTESIAN_POINT ( 'NONE',  ( 5.731347020009612645E-17, 3.842444444444443441, 0.3119999999999999996 ) ) ;
#3849 = EDGE_CURVE ( 'NONE', #1715, #11042, #21758, .T. ) ;
#3850 = CARTESIAN_POINT ( 'NONE',  ( 0.2206173157302028787, 4.634111111262843252, 0.2206173157302027954 ) ) ;
#3851 = EDGE_CURVE ( 'NONE', #21992, #12983, #5009, .T. ) ;
#3852 = CARTESIAN_POINT ( 'NONE',  ( 0.1993543840281266633, 5.179250000075866112, -0.1993543840281266910 ) ) ;
#3853 = CARTESIAN_POINT ( 'NONE',  ( 0.1292346314604056745, 0.4173611111111109051, -0.3119999999999999996 ) ) ;
#3854 = ORIENTED_EDGE ( 'NONE', *, *, #2438, .T. ) ;
#3855 = CARTESIAN_POINT ( 'NONE',  ( 7.256325792998745354E-13, 0.06073895945496885634, 0.3102389594549692098 ) ) ;
#3856 = ORIENTED_EDGE ( 'NONE', *, *, #6472, .T. ) ;
#3857 = PERSON_AND_ORGANIZATION_ROLE ( 'classification_officer' ) ;
#3858 = VERTEX_POINT ( 'NONE', #16174 ) ;
#3859 =( BOUNDED_CURVE ( )  B_SPLINE_CURVE ( 2, ( #18526, #16937, #18407, #1816, #15001, #1585, #20597, #13184, #9260 ),
 .UNSPECIFIED., .F., .T. ) 
 B_SPLINE_CURVE_WITH_KNOTS ( ( 3, 2, 2, 2, 3 ),
 ( 0.4062499999999999445, 0.4166666666666667407, 0.4270833333333333703, 0.4375000000000001110, 0.4479166666666667407 ),
 .UNSPECIFIED. ) 
 CURVE ( )  GEOMETRIC_REPRESENTATION_ITEM ( )  RATIONAL_B_SPLINE_CURVE ( ( 1.000000000000000444, 0.9238795325112862944, 1.000000000000000000, 0.9238795325112867385, 1.000000000000000000, 0.9238795325112867385, 1.000000000000000000, 0.9238795325112862944, 1.000000000000000444 ) ) 
 REPRESENTATION_ITEM ( '' )  );
#3860 = CARTESIAN_POINT ( 'NONE',  ( 0.4621664414996921044, 0.2744339579550159058, 0.05971062996526297489 ) ) ;
#3861 = CARTESIAN_POINT ( 'NONE',  ( 0.1167790944451424368, 5.148000000075865223, 0.2819296736111110424 ) ) ;
#3862 =( BOUNDED_CURVE ( )  B_SPLINE_CURVE ( 2, ( #1242, #19650, #14168, #13814, #6604, #15997, #16118, #21367, #17704 ),
 .UNSPECIFIED., .F., .T. ) 
 B_SPLINE_CURVE_WITH_KNOTS ( ( 3, 2, 2, 2, 3 ),
 ( 0.07291666666666669905, 0.08333333333333332871, 0.09374999999999994449, 0.1041666666666666852, 0.1145833333333333148 ),
 .UNSPECIFIED. ) 
 CURVE ( )  GEOMETRIC_REPRESENTATION_ITEM ( )  RATIONAL_B_SPLINE_CURVE ( ( 1.000000000000000222, 0.9238795325112864054, 1.000000000000000000, 0.9238795325112867385, 1.000000000000000000, 0.9238795325112867385, 1.000000000000000000, 0.9238795325112871826, 0.9999999999999995559 ) ) 
 REPRESENTATION_ITEM ( '' )  );
#3863 = CARTESIAN_POINT ( 'NONE',  ( -0.2819296736111110979, 3.974388888964754951, -0.1167790944451422980 ) ) ;
#3864 = VECTOR ( 'NONE', #2643, 39.37007874015748854 ) ;
#3865 = CARTESIAN_POINT ( 'NONE',  ( 0.2999766478522543633, 4.416353878536761535, 0.08855854222874144643 ) ) ;
#3866 = CARTESIAN_POINT ( 'NONE',  ( 0.000000000000000000, 0.1199999999999999956, 0.000000000000000000 ) ) ;
#3867 = CARTESIAN_POINT ( 'NONE',  ( -0.2764156081756484196, -0.1144950937579609362, 0.03625000000000147549 ) ) ;
#3868 = CARTESIAN_POINT ( 'NONE',  ( 0.2819296736111110424, 0.4347222221463555858, 0.1167790944451424923 ) ) ;
#3869 = CARTESIAN_POINT ( 'NONE',  ( -0.1144950937579609779, 0.2764156081756484196, 0.1959722222222249899 ) ) ;
#3870 = CARTESIAN_POINT ( 'NONE',  ( 5.178964085587577574E-17, 4.991750000075866112, 0.2819296736111110979 ) ) ;
#3871 = CARTESIAN_POINT ( 'NONE',  ( -0.3236067977499790249, 0.4339285712334866041, 0.2351141009169892271 ) ) ;
#3872 = CARTESIAN_POINT ( 'NONE',  ( 0.1167790944451422702, 4.891055555631421470, -0.2819296736111110424 ) ) ;
#3873 = FACE_OUTER_BOUND ( 'NONE', #2853, .T. ) ;
#3874 = CARTESIAN_POINT ( 'NONE',  ( 0.006049195330367759457, 4.877003847587220164, -0.3119499012820716177 ) ) ;
#3875 = CARTESIAN_POINT ( 'NONE',  ( 1.573500000000000343, -3.414809992080329023E-17, -0.3524999999999999800 ) ) ;
#3876 = CARTESIAN_POINT ( 'NONE',  ( 0.2800968539712072602, -5.145295735006237905E-17, 0.3917635206378741186 ) ) ;
#3877 = CARTESIAN_POINT ( 'NONE',  ( -0.1292346314604056745, 4.540361111111110404, -0.3119999999999999996 ) ) ;
#3878 = CARTESIAN_POINT ( 'NONE',  ( -0.2819296736111110424, 3.856333333409199149, 0.1167790944451424923 ) ) ;
#3879 = CARTESIAN_POINT ( 'NONE',  ( 0.3119999999999999996, 0.3444444442927114824, 0.000000000000000000 ) ) ;
#3880 = CARTESIAN_POINT ( 'NONE',  ( 0.002644507750069672973, 4.988201934502406232, -0.3119903920917703743 ) ) ;
#3881 = LINE ( 'NONE', #20705, #16782 ) ;
#3882 = VECTOR ( 'NONE', #7538, 39.37007874015748143 ) ;
#3883 = CARTESIAN_POINT ( 'NONE',  ( 0.3109270811063121753, 4.584793454335284402, 0.02585305464956524218 ) ) ;
#3884 = DIRECTION ( 'NONE',  ( 0.000000000000000000, -1.000000000000000000, 0.000000000000000000 ) ) ;
#3885 = CARTESIAN_POINT ( 'NONE',  ( -3.385114897866767815E-17, -0.2764156081756484196, 0.4355555555555601921 ) ) ;
#3886 = CARTESIAN_POINT ( 'NONE',  ( -0.2206173157302028787, 0.3861111111111107386, 0.2206173157302027954 ) ) ;
#3887 = CARTESIAN_POINT ( 'NONE',  ( 1.222470958122163998, 0.000000000000000000, -0.6167782587447089293 ) ) ;
#3888 = ORIENTED_EDGE ( 'NONE', *, *, #20650, .T. ) ;
#3889 = CIRCLE ( 'NONE', #17144, 0.01875000000000003400 ) ;
#3890 = CARTESIAN_POINT ( 'NONE',  ( 0.2233192592356399997, 0.3794642856167432798, -0.3073725909049500049 ) ) ;
#3891 = CIRCLE ( 'NONE', #20639, 0.3149999999999999467 ) ;
#3892 = CARTESIAN_POINT ( 'NONE',  ( -0.1167790944451422702, 0.2194444443685777957, -0.2819296736111110424 ) ) ;
#3893 = CARTESIAN_POINT ( 'NONE',  ( -2.147421952792136087E-16, 0.9967515475838637506, 0.000000000000000000 ) ) ;
#3894 = CARTESIAN_POINT ( 'NONE',  ( 0.4620259694561523744, -0.2880908832651558615, 0.04413116910601658921 ) ) ;
#3895 = CC_DESIGN_PERSON_AND_ORGANIZATION_ASSIGNMENT ( #16725, #13441, ( #3736 ) ) ;
#3896 = CARTESIAN_POINT ( 'NONE',  ( 0.1395639791202929747, 0.4606885764509979220, 0.4108348780186336091 ) ) ;
#3897 = CARTESIAN_POINT ( 'NONE',  ( 0.1954553509668047195, 0.1954553509668046085, 0.2966666666666701313 ) ) ;
#3898 = ORIENTED_EDGE ( 'NONE', *, *, #15758, .T. ) ;
#3899 = DIRECTION ( 'NONE',  ( 0.000000000000000000, 0.000000000000000000, -1.000000000000000000 ) ) ;
#3900 = CARTESIAN_POINT ( 'NONE',  ( 0.4687500000000003886, 0.1119035383512243936, 0.4216345187268149552 ) ) ;
#3901 = CARTESIAN_POINT ( 'NONE',  ( 0.2206173157302028232, 0.2472222222222218435, -0.2206173157302028232 ) ) ;
#3902 = CARTESIAN_POINT ( 'NONE',  ( -1.910449006669871087E-17, 5.259111111111110404, -0.3119999999999999996 ) ) ;
#3903 =( REPRESENTATION_RELATIONSHIP ('NONE','NONE', #4490, #1861 ) REPRESENTATION_RELATIONSHIP_WITH_TRANSFORMATION ( #3674 )SHAPE_REPRESENTATION_RELATIONSHIP( ) );
#3904 = ORIENTED_EDGE ( 'NONE', *, *, #22862, .F. ) ;
#3905 = CARTESIAN_POINT ( 'NONE',  ( -0.1993543840281266910, 4.137583333409199149, -0.1993543840281266910 ) ) ;
#3906 = DIRECTION ( 'NONE',  ( 0.000000000000000000, 0.000000000000000000, -1.000000000000000000 ) ) ;
#3907 = CARTESIAN_POINT ( 'NONE',  ( 0.3125000000000000000, -5.740531871003217465E-17, 0.2063888888888918416 ) ) ;
#3908 = ORIENTED_EDGE ( 'NONE', *, *, #15981, .T. ) ;
#3909 = DIRECTION ( 'NONE',  ( 1.000000000000000000, 0.000000000000000000, 0.000000000000000000 ) ) ;
#3910 = CARTESIAN_POINT ( 'NONE',  ( -0.1993543840281266910, 4.957027777853642903, -0.1993543840281266910 ) ) ;
#3911 = AXIS2_PLACEMENT_3D ( 'NONE', #14887, #18652, #22306 ) ;
#3912 = CARTESIAN_POINT ( 'NONE',  ( 0.08148075347861075124, 4.184984852033682756, 0.3039166203302874902 ) ) ;
#3913 = VECTOR ( 'NONE', #9263, 39.37007874015748143 ) ;
#3914 =( NAMED_UNIT ( * ) SI_UNIT ( $, .STERADIAN. ) SOLID_ANGLE_UNIT ( ) );
#3915 = DIRECTION ( 'NONE',  ( 0.000000000000000000, 0.000000000000000000, -1.000000000000000000 ) ) ;
#3916 = CARTESIAN_POINT ( 'NONE',  ( 0.2969103404914450461, -0.03343391069991762110, -0.08748023474661176246 ) ) ;
#3917 = CARTESIAN_POINT ( 'NONE',  ( -1.726321361862525858E-17, 4.727861111186976828, -0.2819296736111110979 ) ) ;
#3918 = DATE_AND_TIME ( #3798, #617 ) ;
#3919 = CARTESIAN_POINT ( 'NONE',  ( -8.893442360197089595E-05, 4.043835722953997625, -0.3120000002135276396 ) ) ;
#3920 = CARTESIAN_POINT ( 'NONE',  ( -0.1144950937579609918, -0.2764156081756484196, -0.005416666666665556629 ) ) ;
#3921 = CARTESIAN_POINT ( 'NONE',  ( -0.1167790944451424368, 0.5874999999241333759, 0.2819296736111110424 ) ) ;
#3922 = ORIENTED_EDGE ( 'NONE', *, *, #1615, .T. ) ;
#3923 = CARTESIAN_POINT ( 'NONE',  ( 0.2819296736111110979, 0.3270833332574666907, 0.000000000000000000 ) ) ;
#3924 = CARTESIAN_POINT ( 'NONE',  ( 0.000000000000000000, 5.384999999999999787, 0.000000000000000000 ) ) ;
#3925 = FACE_BOUND ( 'NONE', #15227, .T. ) ;
#3926 = CARTESIAN_POINT ( 'NONE',  ( -0.1236067977499790416, 0.2357142857142856818, 0.3804226065180614236 ) ) ;
#3927 = CARTESIAN_POINT ( 'NONE',  ( -0.3155070326520293400, 0.1306872919485614903, -0.1078472222222221499 ) ) ;
#3928 = EDGE_CURVE ( 'NONE', #14964, #2709, #17830, .T. ) ;
#3929 = CARTESIAN_POINT ( 'NONE',  ( -0.05483022876052533884, -0.5228926224321407412, 0.05347271648849222930 ) ) ;
#3930 = CONICAL_SURFACE ( 'NONE', #17558, 0.2041999999999999926, 0.7853981633974621568 ) ;
#3931 = DIRECTION ( 'NONE',  ( 0.8660254037844364872, 0.000000000000000000, -0.5000000000000038858 ) ) ;
#3932 = CARTESIAN_POINT ( 'NONE',  ( -0.2819296736111110979, 0.1743055554796889284, -3.452642723725051716E-17 ) ) ;
#3933 = CARTESIAN_POINT ( 'NONE',  ( -0.2819296736111110979, 0.06319444436857780956, -3.452642723725051716E-17 ) ) ;
#3934 = CIRCLE ( 'NONE', #5872, 1.243000000000000105 ) ;
#3935 = CARTESIAN_POINT ( 'NONE',  ( -0.2819296736111110424, 4.363277777853643791, -0.1167790944451423119 ) ) ;
#3936 = CARTESIAN_POINT ( 'NONE',  ( 0.2472135954999579166, 0.09464285694777235802, 0.3402603233408160732 ) ) ;
#3937 = CARTESIAN_POINT ( 'NONE',  ( 0.1993543840281267465, 4.832027777853643791, 0.1993543840281266633 ) ) ;
#3938 = CARTESIAN_POINT ( 'NONE',  ( -0.1993543840281266910, 4.345916666742532186, -0.1993543840281266910 ) ) ;
#3939 = CARTESIAN_POINT ( 'NONE',  ( 0.000000000000000000, 3.700000000000000622, 0.000000000000000000 ) ) ;
#3940 = CARTESIAN_POINT ( 'NONE',  ( -0.01172578639831971595, 0.5344959914317446437, 0.04874733047933995506 ) ) ;
#3941 = CARTESIAN_POINT ( 'NONE',  ( 0.1292346314604058410, 4.075083333485065573, 0.3119999999999998885 ) ) ;
#3942 = DIRECTION ( 'NONE',  ( 8.659560562355001884E-17, 0.7071067811865416886, -0.7071067811865531239 ) ) ;
#3943 = ORIENTED_EDGE ( 'NONE', *, *, #9327, .T. ) ;
#3944 = EDGE_CURVE ( 'NONE', #23326, #19970, #10689, .T. ) ;
#3945 = VECTOR ( 'NONE', #7374, 39.37007874015748143 ) ;
#3946 = EDGE_CURVE ( 'NONE', #21142, #10130, #17137, .T. ) ;
#3947 = APPROVAL_DATE_TIME ( #20647, #6729 ) ;
#3948 = CARTESIAN_POINT ( 'NONE',  ( 2.283224615330811780, 2.690142902515283208, -2.474227944919804578 ) ) ;
#3949 = FACE_OUTER_BOUND ( 'NONE', #12550, .T. ) ;
#3950 = EDGE_LOOP ( 'NONE', ( #19649, #1450, #14644, #15470 ) ) ;
#3951 = CARTESIAN_POINT ( 'NONE',  ( 1.910449006669871087E-17, 0.4138888887371559577, -0.3119999999999999996 ) ) ;
#3952 = ORIENTED_EDGE ( 'NONE', *, *, #16480, .T. ) ;
#3953 = CARTESIAN_POINT ( 'NONE',  ( 2.361000000000004206, 0.000000000000000000, -2.201288568297000925 ) ) ;
#3954 = DIRECTION ( 'NONE',  ( -0.8660254037844360431, 0.000000000000000000, -0.5000000000000043299 ) ) ;
#3955 = CARTESIAN_POINT ( 'NONE',  ( -0.3613381517857143232, -0.04553571438325666049, -0.1174058825155741004 ) ) ;
#3956 = LINE ( 'NONE', #11165, #14756 ) ;
#3957 = EDGE_CURVE ( 'NONE', #6883, #2823, #8305, .T. ) ;
#3958 = VERTEX_POINT ( 'NONE', #424 ) ;
#3959 = CARTESIAN_POINT ( 'NONE',  ( 0.3613381517857143232, 0.1508928570453147155, 0.1174058825155741975 ) ) ;
#3960 = CARTESIAN_POINT ( 'NONE',  ( 0.008081987039794995969, 0.9548081934128058723, 3.210421403429992271 ) ) ;
#3961 = CARTESIAN_POINT ( 'NONE',  ( -0.2764156081756484196, -0.1144950937579609362, 0.4251388888888933959 ) ) ;
#3962 = CARTESIAN_POINT ( 'NONE',  ( 0.1167790944451422702, 4.002166666742532186, -0.2819296736111110424 ) ) ;
#3963 = CARTESIAN_POINT ( 'NONE',  ( -0.07891297495569016274, 0.03366361305084811933, 0.2724293070475350964 ) ) ;
#3964 = CARTESIAN_POINT ( 'NONE',  ( -0.1292346314604020385, 4.838972222222222008, 0.3120000000000036078 ) ) ;
#3965 = CARTESIAN_POINT ( 'NONE',  ( 5.731347020009612645E-17, 3.897999999999999243, 0.3119999999999999996 ) ) ;
#3966 = CARTESIAN_POINT ( 'NONE',  ( 0.2206173157302027954, 4.759111111262843252, -0.2206173157302028232 ) ) ;
#3967 = CARTESIAN_POINT ( 'NONE',  ( 5.178964085587577574E-17, 4.936194444520309865, 0.2819296736111110979 ) ) ;
#3968 = CARTESIAN_POINT ( 'NONE',  ( -0.1167790944451423535, 4.363277777853642903, 0.2819296736111110424 ) ) ;
#3969 = CARTESIAN_POINT ( 'NONE',  ( -0.1547861949055390485, 3.900357038476919058, 0.2724574402709006860 ) ) ;
#3970 = CARTESIAN_POINT ( 'NONE',  ( 0.2233192592356399164, 0.1258928570453146933, 0.3073725909049500604 ) ) ;
#3971 = VERTEX_POINT ( 'NONE', #7742 ) ;
#3972 = ORIENTED_EDGE ( 'NONE', *, *, #10217, .T. ) ;
#3973 = PERSON_AND_ORGANIZATION ( #15518, #2538 ) ;
#3974 = CARTESIAN_POINT ( 'NONE',  ( 0.1306872919485614071, -0.3155070326520293955, 0.4164583333333380377 ) ) ;
#3975 = CARTESIAN_POINT ( 'NONE',  ( 5.178964085587577574E-17, 5.033416666742532186, 0.2819296736111110979 ) ) ;
#3976 = CARTESIAN_POINT ( 'NONE',  ( 0.1167790944451424506, 3.773000000075866112, 0.2819296736111110424 ) ) ;
#3977 = CARTESIAN_POINT ( 'NONE',  ( 0.04072223948701583079, 4.406056745573514455, 0.3100004575725601730 ) ) ;
#3978 = EDGE_CURVE ( 'NONE', #20894, #5886, #7739, .T. ) ;
#3979 = CARTESIAN_POINT ( 'NONE',  ( 0.2021572709300329673, -0.4370510722512370161, 0.07439726544913842499 ) ) ;
#3980 = CARTESIAN_POINT ( 'NONE',  ( -3.385114897866767815E-17, -0.2764156081756484196, 0.3244444444444482545 ) ) ;
#3981 = CARTESIAN_POINT ( 'NONE',  ( 0.1993543840281266910, 0.5562499999241333759, -0.1993543840281266910 ) ) ;
#3982 = CARTESIAN_POINT ( 'NONE',  ( -3.385114897866767815E-17, -0.2764156081756484196, -0.06444444444444379083 ) ) ;
#3983 = CARTESIAN_POINT ( 'NONE',  ( -0.1993543840281266910, 4.859805555631421470, -0.1993543840281266910 ) ) ;
#3984 = CARTESIAN_POINT ( 'NONE',  ( -0.006583943204589224121, -0.5374646359837778054, 0.05971082423030150271 ) ) ;
#3985 = VECTOR ( 'NONE', #3240, 39.37007874015748854 ) ;
#3986 = CARTESIAN_POINT ( 'NONE',  ( -1.726321361862525858E-17, 4.838972222298088433, -0.2819296736111110979 ) ) ;
#3987 = DIRECTION ( 'NONE',  ( 0.000000000000000000, 0.000000000000000000, 1.000000000000000000 ) ) ;
#3988 = CARTESIAN_POINT ( 'NONE',  ( 0.2249574224929273558, 4.856505608673026053, 0.2162428277538668564 ) ) ;
#3989 = DIRECTION ( 'NONE',  ( 0.000000000000000000, 1.000000000000000000, 0.000000000000000000 ) ) ;
#3990 = FACE_OUTER_BOUND ( 'NONE', #11301, .T. ) ;
#3991 = CARTESIAN_POINT ( 'NONE',  ( 0.3119999999999999996, 4.526472222222221120, -0.1292346314604056745 ) ) ;
#3992 = CARTESIAN_POINT ( 'NONE',  ( 0.1993543840281266633, 3.776472222298087988, -0.1993543840281266910 ) ) ;
#3993 = LINE ( 'NONE', #23081, #24091 ) ;
#3994 = DIRECTION ( 'NONE',  ( 0.000000000000000000, 0.000000000000000000, -1.000000000000000000 ) ) ;
#3995 = ORIENTED_EDGE ( 'NONE', *, *, #7681, .T. ) ;
#3996 = CARTESIAN_POINT ( 'NONE',  ( 0.4500000000000003442, -0.2598076211353317899, 0.3779506566538943235 ) ) ;
#3997 = ORIENTED_EDGE ( 'NONE', *, *, #2272, .F. ) ;
#3998 =( BOUNDED_SURFACE ( )  B_SPLINE_SURFACE ( 3, 1, ( 
 ( #12143, #21144 ),
 ( #14072, #1143 ),
 ( #8580, #6746 ),
 ( #23077, #2732 ) ),
 .UNSPECIFIED., .F., .F., .F. ) 
 B_SPLINE_SURFACE_WITH_KNOTS ( ( 4, 4 ),
 ( 2, 2 ),
 ( 0.000000000000000000, 1.000000000000000000 ),
 ( 0.000000000000000000, 1.000000000000000000 ),
 .UNSPECIFIED. ) 
 GEOMETRIC_REPRESENTATION_ITEM ( )  RATIONAL_B_SPLINE_SURFACE ( (
 ( 1.000000000000000000, 1.000000000000000000),
 ( 0.3333333333333338144, 0.3333333333333338144),
 ( 0.3333333333333338144, 0.3333333333333338144),
 ( 1.000000000000000000, 1.000000000000000000) ) ) 
 REPRESENTATION_ITEM ( '' )  SURFACE ( )  );
#3999 =( BOUNDED_CURVE ( )  B_SPLINE_CURVE ( 2, ( #17152, #12163, #442, #7873, #15323, #22753, #20924, #6044, #4218 ),
 .UNSPECIFIED., .F., .F. ) 
 B_SPLINE_CURVE_WITH_KNOTS ( ( 3, 2, 2, 2, 3 ),
 ( 0.4017857142857142461, 0.4062500000000000000, 0.4107142857142856984, 0.4151785714285715079, 0.4196428571428572063 ),
 .UNSPECIFIED. ) 
 CURVE ( )  GEOMETRIC_REPRESENTATION_ITEM ( )  RATIONAL_B_SPLINE_CURVE ( ( 1.000000000000000888, 0.9238795325112857393, 1.000000000000000000, 0.9238795325112867385, 1.000000000000000000, 0.9238795325112867385, 1.000000000000000000, 0.9238795325112857393, 1.000000000000000888 ) ) 
 REPRESENTATION_ITEM ( '' )  );
#4000 = CARTESIAN_POINT ( 'NONE',  ( -2.918002456435568987E-09, 4.127166543308980806, 0.3119999999999999996 ) ) ;
#4001 = VECTOR ( 'NONE', #17256, 39.37007874015748143 ) ;
#4002 = CARTESIAN_POINT ( 'NONE',  ( 0.0003241969039724112056, 4.654935146396195655, -0.3120000004149252049 ) ) ;
#4003 = CARTESIAN_POINT ( 'NONE',  ( 0.3155070326520292845, -5.795770164686806123E-17, -0.07312499999999920453 ) ) ;
#4004 = ORIENTED_EDGE ( 'NONE', *, *, #11728, .T. ) ;
#4005 = EDGE_CURVE ( 'NONE', #11906, #20538, #6564, .T. ) ;
#4006 = CARTESIAN_POINT ( 'NONE',  ( 0.3039609707416114359, 4.309972269864218219, -0.08137645367071676128 ) ) ;
#4007 = CARTESIAN_POINT ( 'NONE',  ( 0.2072783878431551374, 5.137695445002894878, 0.2242608243709702798 ) ) ;
#4008 = ADVANCED_FACE ( 'NONE', ( #5790, #13254 ), #11175, .F. ) ;
#4009 = VERTEX_POINT ( 'NONE', #2019 ) ;
#4010 = CARTESIAN_POINT ( 'NONE',  ( 0.2233192592356399997, 0.3080357141881718275, -0.3073725909049500049 ) ) ;
#4011 = CARTESIAN_POINT ( 'NONE',  ( -0.2819296736111110979, 0.3999999999241333759, 0.1167790944451422425 ) ) ;
#4012 = DIRECTION ( 'NONE',  ( -0.000000000000000000, -1.000000000000000000, -0.000000000000000000 ) ) ;
#4013 = CARTESIAN_POINT ( 'NONE',  ( 0.2728372834934218449, 0.3240490730395221286, -1.173104893136099891 ) ) ;
#4014 = CARTESIAN_POINT ( 'NONE',  ( 3.820898013339742174E-17, 5.384999999999999787, 0.3119999999999999996 ) ) ;
#4015 = CARTESIAN_POINT ( 'NONE',  ( -0.1954553509668046640, 0.1954553509668046918, 0.1438888888888912032 ) ) ;
#4016 = CARTESIAN_POINT ( 'NONE',  ( 0.000000000000000000, 5.072999999999999510, 0.000000000000000000 ) ) ;
#4017 = DIRECTION ( 'NONE',  ( -0.000000000000000000, -1.000000000000000000, -0.000000000000000000 ) ) ;
#4018 = CARTESIAN_POINT ( 'NONE',  ( 0.2206173157302027676, 0.3444444444444440534, 0.2206173157302028787 ) ) ;
#4019 = CARTESIAN_POINT ( 'NONE',  ( -0.2206173157302027676, 5.224388888888887195, 0.2206173157302028787 ) ) ;
#4020 = VECTOR ( 'NONE', #13628, 39.37007874015748854 ) ;
#4021 = CARTESIAN_POINT ( 'NONE',  ( 0.1167790944451422702, 4.238277777853643791, -0.2819296736111110424 ) ) ;
#4022 = DIRECTION ( 'NONE',  ( 0.000000000000000000, -0.9961946980917454342, -0.08715574274765833240 ) ) ;
#4023 = CARTESIAN_POINT ( 'NONE',  ( -0.4366234456863259394, 1.999640111863030478, -2.684082427924094016 ) ) ;
#4024 = ORIENTED_EDGE ( 'NONE', *, *, #22145, .T. ) ;
#4025 = VERTEX_POINT ( 'NONE', #15073 ) ;
#4026 = CARTESIAN_POINT ( 'NONE',  ( 0.3125000000000000555, -5.740531871003217465E-17, 0.1508333333333358728 ) ) ;
#4027 = CARTESIAN_POINT ( 'NONE',  ( 0.1993543840281266633, 5.054250000075865223, -0.1993543840281266910 ) ) ;
#4028 = CARTESIAN_POINT ( 'NONE',  ( 0.04074832584215749842, 4.183841529647392754, 0.3119999987872715264 ) ) ;
#4029 = SHAPE_REPRESENTATION_RELATIONSHIP ( 'NONE' , 'NONE' ,  #12001, #14347 ) ;
#4030 = CARTESIAN_POINT ( 'NONE',  ( -0.1954553509668046640, 0.1954553509668046918, -0.1408333333333332826 ) ) ;
#4031 = CARTESIAN_POINT ( 'NONE',  ( 0.2819296736111111534, 4.335500000075866112, 0.1167790944451422563 ) ) ;
#4032 = DATE_AND_TIME ( #18790, #637 ) ;
#4033 = DIRECTION ( 'NONE',  ( -0.000000000000000000, -0.000000000000000000, -1.000000000000000000 ) ) ;
#4034 = LINE ( 'NONE', #19151, #11247 ) ;
#4035 = CARTESIAN_POINT ( 'NONE',  ( -0.1167790944451424368, 0.4208333332574665797, 0.2819296736111110424 ) ) ;
#4036 = ORIENTED_EDGE ( 'NONE', *, *, #3192, .T. ) ;
#4037 = CARTESIAN_POINT ( 'NONE',  ( 0.2819296736111110424, 0.5458333332574666352, 0.1167790944451424923 ) ) ;
#4038 = CARTESIAN_POINT ( 'NONE',  ( 0.2800968539712072602, -5.145295735006237905E-17, 0.3917635206378741186 ) ) ;
#4039 = DIRECTION ( 'NONE',  ( 0.000000000000000000, 0.000000000000000000, -1.000000000000000000 ) ) ;
#4040 = CARTESIAN_POINT ( 'NONE',  ( -0.4000000000000000222, 0.1499999999999999667, -4.898587196589413075E-17 ) ) ;
#4041 = CARTESIAN_POINT ( 'NONE',  ( 0.2230971623002954429, 0.2230971623002953319, 0.1525694444444466169 ) ) ;
#4042 = CARTESIAN_POINT ( 'NONE',  ( -0.3886748462736269172, -0.3298755754955817743, 0.06108448616841026524 ) ) ;
#4043 = FACE_OUTER_BOUND ( 'NONE', #17823, .T. ) ;
#4044 = CARTESIAN_POINT ( 'NONE',  ( 0.2819296736111110979, 0.2020833332574666907, 0.000000000000000000 ) ) ;
#4045 = CARTESIAN_POINT ( 'NONE',  ( 0.1993543840281266910, 0.3201388888130222710, -0.1993543840281266910 ) ) ;
#4046 = CARTESIAN_POINT ( 'NONE',  ( -0.1993543840281266910, 4.359805555631421470, -0.1993543840281266910 ) ) ;
#4047 = CARTESIAN_POINT ( 'NONE',  ( 0.1236067977499789028, 0.3767857140906294422, 0.3804226065180614791 ) ) ;
#4048 = CARTESIAN_POINT ( 'NONE',  ( 0.2819296736111110979, 4.950083333409199149, -3.452642723725051716E-17 ) ) ;
#4049 = CARTESIAN_POINT ( 'NONE',  ( 0.2819296736111110979, 4.439666666742532186, -0.1167790944451423396 ) ) ;
#4050 = EDGE_CURVE ( 'NONE', #5967, #4025, #15493, .T. ) ;
#4051 = DIRECTION ( 'NONE',  ( 0.000000000000000000, 0.000000000000000000, -1.000000000000000000 ) ) ;
#4052 = CARTESIAN_POINT ( 'NONE',  ( -0.3616234456863257618, 4.559812086079793048, -2.727383698113316157 ) ) ;
#4053 = CARTESIAN_POINT ( 'NONE',  ( 0.1292346314604056190, 4.095916666818398610, -0.3119999999999999996 ) ) ;
#4054 = AXIS2_PLACEMENT_3D ( 'NONE', #17588, #21125, #15999 ) ;
#4055 = LINE ( 'NONE', #18815, #14983 ) ;
#4056 = EDGE_CURVE ( 'NONE', #412, #12482, #17051, .T. ) ;
#4057 = VERTEX_POINT ( 'NONE', #17009 ) ;
#4058 = PERSON_AND_ORGANIZATION ( #15518, #2538 ) ;
#4059 = CARTESIAN_POINT ( 'NONE',  ( 0.1209188320989911664, 0.2598538660581671822, 0.3981211010572119902 ) ) ;
#4060 = DIRECTION ( 'NONE',  ( 1.000000000000000000, 0.000000000000000000, -0.000000000000000000 ) ) ;
#4061 = CARTESIAN_POINT ( 'NONE',  ( -1.054647954922321762E-07, 4.988277780858759947, -0.3119999999999820695 ) ) ;
#4062 = VERTEX_POINT ( 'NONE', #16774 ) ;
#4063 = CARTESIAN_POINT ( 'NONE',  ( -0.1292346314604058410, 0.6048611109593783342, 0.3119999999999998885 ) ) ;
#4064 = ORIENTED_EDGE ( 'NONE', *, *, #23173, .F. ) ;
#4065 = CARTESIAN_POINT ( 'NONE',  ( 0.000000000000000000, 5.384999999999999787, 0.000000000000000000 ) ) ;
#4066 = CARTESIAN_POINT ( 'NONE',  ( -1.910449006669871087E-17, 4.647999999999998799, -0.3119999999999999996 ) ) ;
#4067 = CARTESIAN_POINT ( 'NONE',  ( 0.3146586916146184576, 4.752112305768198652, 0.001375812536115708813 ) ) ;
#4068 = AXIS2_PLACEMENT_3D ( 'NONE', #10430, #1627, #12622 ) ;
#4069 = CARTESIAN_POINT ( 'NONE',  ( 2.326421213736078119E-17, 0.01160714275960046671, -0.3799334167787516425 ) ) ;
#4070 = FACE_OUTER_BOUND ( 'NONE', #8440, .T. ) ;
#4071 = VERTEX_POINT ( 'NONE', #9576 ) ;
#4072 = CARTESIAN_POINT ( 'NONE',  ( -0.2923287055106771337, 0.3401785713310290227, 0.2123892367102619971 ) ) ;
#4073 = CARTESIAN_POINT ( 'NONE',  ( -2.187612651176460788E-16, 0.5196152422706634688, 0.3779506566538943790 ) ) ;
#4074 = CARTESIAN_POINT ( 'NONE',  ( -0.2284009101814420406, 4.675474525268722203, 0.2125530810637378254 ) ) ;
#4075 = CARTESIAN_POINT ( 'NONE',  ( -0.1167790944451423535, 3.974388888964754063, 0.2819296736111110424 ) ) ;
#4076 = CARTESIAN_POINT ( 'NONE',  ( -0.3068695747081881531, -0.3531079105191464729, 0.4306248051561444301 ) ) ;
#4077 = CARTESIAN_POINT ( 'NONE',  ( -1.062695237341364068E-12, 5.118312382271687611, 0.3086920601714014945 ) ) ;
#4078 = EDGE_CURVE ( 'NONE', #16166, #13675, #101, .T. ) ;
#4079 = CARTESIAN_POINT ( 'NONE',  ( 0.4035778243552766709, 3.745586516788660170, -0.07105710959332679766 ) ) ;
#4080 = CARTESIAN_POINT ( 'NONE',  ( 0.2206173157302028787, 4.745222222373954857, 0.2206173157302027954 ) ) ;
#4081 = CARTESIAN_POINT ( 'NONE',  ( 0.1167790944451422702, 4.849388888964755395, -0.2819296736111110979 ) ) ;
#4082 = ORIENTED_EDGE ( 'NONE', *, *, #22697, .T. ) ;
#4083 = CARTESIAN_POINT ( 'NONE',  ( -0.2819296736111110424, 4.245222222298087544, 0.1167790944451424923 ) ) ;
#4084 = ORIENTED_EDGE ( 'NONE', *, *, #22172, .F. ) ;
#4085 = EDGE_CURVE ( 'NONE', #9548, #6543, #16466, .T. ) ;
#4086 = EDGE_LOOP ( 'NONE', ( #10118, #5738, #15930, #16495 ) ) ;
#4087 = EDGE_LOOP ( 'NONE', ( #3829, #12086, #1304, #10874, #7225, #836 ) ) ;
#4088 = PERSON_AND_ORGANIZATION_ROLE ( 'design_owner' ) ;
#4089 = DIRECTION ( 'NONE',  ( 0.000000000000000000, 1.000000000000000000, 0.000000000000000000 ) ) ;
#4090 = DIRECTION ( 'NONE',  ( -0.8660254037844383745, 0.000000000000000000, -0.5000000000000004441 ) ) ;
#4091 = LOCAL_TIME ( 21, 9, 13.00000000000000000, #11546 ) ;
#4092 = CARTESIAN_POINT ( 'NONE',  ( 0.1993543840281267465, 3.943138888964754951, 0.1993543840281266633 ) ) ;
#4093 = CARTESIAN_POINT ( 'NONE',  ( 0.2839364041945253159, 4.422813250354537651, -0.1344124572274522367 ) ) ;
#4094 = CARTESIAN_POINT ( 'NONE',  ( 0.1144950937579611444, 0.2764156081756483641, 0.3556944444444484210 ) ) ;
#4095 = EDGE_CURVE ( 'NONE', #11153, #14969, #6920, .T. ) ;
#4096 = B_SPLINE_CURVE_WITH_KNOTS ( 'NONE', 3,
 ( #18823, #2369, #5535, #20890, #18948, #11156 ),
 .UNSPECIFIED., .F., .F.,
 ( 4, 2, 4 ),
 ( 0.008885579728328409088, 0.01010732856524649767, 0.01132907740216458452 ),
 .UNSPECIFIED. ) ;
#4097 = CARTESIAN_POINT ( 'NONE',  ( 0.01630689377124411657, 0.06101829741696308818, 0.3105182974169249932 ) ) ;
#4098 = CARTESIAN_POINT ( 'NONE',  ( -0.1144950937579609918, -0.2764156081756484196, 0.2098611111111139960 ) ) ;
#4099 = CARTESIAN_POINT ( 'NONE',  ( 0.1993543840281266355, 0.4312499999241333759, 0.1993543840281267465 ) ) ;
#4100 = CARTESIAN_POINT ( 'NONE',  ( 0.2764156081756484196, -5.077672346800151106E-17, -0.05055555555555477781 ) ) ;
#4101 = CARTESIAN_POINT ( 'NONE',  ( 0.1993543840281267465, 5.054250000075865223, 0.1993543840281266633 ) ) ;
#4102 = CARTESIAN_POINT ( 'NONE',  ( -0.4000000000000000222, 0.4303571426620579898, 0.1299678784931624920 ) ) ;
#4103 = VECTOR ( 'NONE', #9902, 39.37007874015748143 ) ;
#4104 = CARTESIAN_POINT ( 'NONE',  ( 0.1993543840281266633, 4.609805555631420582, -0.1993543840281266910 ) ) ;
#4105 = CARTESIAN_POINT ( 'NONE',  ( -0.2229532752983975630, 0.1767350293216390922, -0.07304505964698700116 ) ) ;
#4106 = CARTESIAN_POINT ( 'NONE',  ( 0.2148596022118366422, 4.856116452778191928, 0.2262407900182530907 ) ) ;
#4107 = CARTESIAN_POINT ( 'NONE',  ( 0.7919466436700954848, 0.05000000000000028727, -2.986000000000000210 ) ) ;
#4108 = CARTESIAN_POINT ( 'NONE',  ( 0.4687500000000014988, 0.2629282712287717150, 0.05975564523638850906 ) ) ;
#4109 = ADVANCED_FACE ( 'NONE', ( #14410 ), #12118, .T. ) ;
#4110 = CARTESIAN_POINT ( 'NONE',  ( -0.1292346314604056745, 4.484805555555555046, -0.3119999999999999996 ) ) ;
#4111 = ADVANCED_FACE ( 'NONE', ( #8551 ), #16114, .T. ) ;
#4112 = CARTESIAN_POINT ( 'NONE',  ( -0.2819296736111110424, 3.800777777853643347, 0.1167790944451424923 ) ) ;
#4113 = CARTESIAN_POINT ( 'NONE',  ( -1.399103805173478513E-17, 0.7678277469539112055, -1.002669935482285890 ) ) ;
#4114 = DIRECTION ( 'NONE',  ( 1.000000000000000000, 0.000000000000000000, 0.000000000000000000 ) ) ;
#4115 = PRODUCT_DEFINITION_FORMATION_WITH_SPECIFIED_SOURCE ( 'ANY', '', #10911, .NOT_KNOWN. ) ;
#4116 = EDGE_LOOP ( 'NONE', ( #13401, #5666, #20362, #22745 ) ) ;
#4117 = FACE_OUTER_BOUND ( 'NONE', #19082, .T. ) ;
#4118 = ORIENTED_EDGE ( 'NONE', *, *, #4412, .F. ) ;
#4119 = ADVANCED_FACE ( 'NONE', ( #5006 ), #21363, .F. ) ;
#4120 = CARTESIAN_POINT ( 'NONE',  ( 0.1129687097031495668, 4.707317419575747230, -0.2914138746359711263 ) ) ;
#4121 = AXIS2_PLACEMENT_3D ( 'NONE', #7019, #21884, #5175 ) ;
#4122 = CARTESIAN_POINT ( 'NONE',  ( -0.2764156081756484196, 0.1144950937579609918, 0.4181944444444490872 ) ) ;
#4123 = CARTESIAN_POINT ( 'NONE',  ( 2.160501146175418441, 2.291712385858714285, -2.201288568297000481 ) ) ;
#4124 = ORIENTED_EDGE ( 'NONE', *, *, #21993, .F. ) ;
#4125 = CARTESIAN_POINT ( 'NONE',  ( 5.178964085587577574E-17, 4.922305555631420582, 0.2819296736111110979 ) ) ;
#4126 = CARTESIAN_POINT ( 'NONE',  ( -0.3613381517857143232, 0.4044642856167432465, -4.425116109941954795E-17 ) ) ;
#4127 = CARTESIAN_POINT ( 'NONE',  ( -0.1167790944451422702, 0.3861111110352444808, -0.2819296736111110424 ) ) ;
#4128 = CARTESIAN_POINT ( 'NONE',  ( 0.2764156081756484196, -5.077672346800151106E-17, -0.09916666666666629215 ) ) ;
#4129 = LINE ( 'NONE', #471, #8431 ) ;
#4130 = CARTESIAN_POINT ( 'NONE',  ( -0.2206173157302028787, 0.1638888888888885287, 0.2206173157302027954 ) ) ;
#4131 = CARTESIAN_POINT ( 'NONE',  ( -0.1144950937579609918, -0.2764156081756484196, 0.2168055555555584712 ) ) ;
#4132 = CARTESIAN_POINT ( 'NONE',  ( -0.2124268279052486941, 5.112105532426204135, 0.2253721325002343290 ) ) ;
#4133 = CARTESIAN_POINT ( 'NONE',  ( 0.4000000000000000222, 0.1053571426620580481, 0.000000000000000000 ) ) ;
#4134 = CARTESIAN_POINT ( 'NONE',  ( -0.3119999999999999996, 0.2159722222222218713, 0.1292346314604056190 ) ) ;
#4135 = CARTESIAN_POINT ( 'NONE',  ( -1.910449006669871087E-17, 5.203555555555554157, -0.3119999999999999996 ) ) ;
#4136 = VECTOR ( 'NONE', #20349, 39.37007874015748143 ) ;
#4137 = CARTESIAN_POINT ( 'NONE',  ( -0.1993543840281266910, 4.304250000075866112, -0.1993543840281266910 ) ) ;
#4138 = CARTESIAN_POINT ( 'NONE',  ( -7.331754493858430024E-07, 4.349360015129621004, 0.3119999999981767358 ) ) ;
#4139 = PLANE ( 'NONE',  #3138 ) ;
#4140 = DIRECTION ( 'NONE',  ( 0.000000000000000000, 0.000000000000000000, -1.000000000000000000 ) ) ;
#4141 = VERTEX_POINT ( 'NONE', #20011 ) ;
#4142 = EDGE_LOOP ( 'NONE', ( #4379, #6293, #19773, #5680 ) ) ;
#4143 = CARTESIAN_POINT ( 'NONE',  ( 0.3999999999999999667, 0.3232142855192008946, -0.1299678784931625197 ) ) ;
#4144 = ADVANCED_FACE ( 'NONE', ( #3298 ), #10752, .F. ) ;
#4145 = CARTESIAN_POINT ( 'NONE',  ( 0.2819296736111110979, 4.713972222298087544, -3.452642723725051716E-17 ) ) ;
#4146 = EDGE_CURVE ( 'NONE', #70, #14521, #19527, .T. ) ;
#4147 = CARTESIAN_POINT ( 'NONE',  ( -0.3613381517857143232, 0.3830357141881717276, -0.1174058825155741143 ) ) ;
#4148 = CARTESIAN_POINT ( 'NONE',  ( -0.03926412191686881603, 5.144338944773434896, -0.3013481353560393816 ) ) ;
#4149 = LINE ( 'NONE', #18665, #7249 ) ;
#4150 = CARTESIAN_POINT ( 'NONE',  ( 0.3860879860166477329, 3.066692553488282957, 2.740461747820544414 ) ) ;
#4151 = EDGE_CURVE ( 'NONE', #9842, #14283, #21120, .T. ) ;
#4152 = VECTOR ( 'NONE', #15002, 39.37007874015748143 ) ;
#4153 = CARTESIAN_POINT ( 'NONE',  ( -0.2819296736111110979, 4.311194444520309865, 0.000000000000000000 ) ) ;
#4154 = COORDINATED_UNIVERSAL_TIME_OFFSET ( 0, 0, .AHEAD. ) ;
#4155 = DIRECTION ( 'NONE',  ( -1.177540334020096294E-17, 0.2588190451025213501, -0.9659258262890680902 ) ) ;
#4156 = CARTESIAN_POINT ( 'NONE',  ( 0.1144950937579611444, 0.2764156081756483641, 0.07791666666666842433 ) ) ;
#4157 = DIRECTION ( 'NONE',  ( -0.000000000000000000, -1.000000000000000000, -0.000000000000000000 ) ) ;
#4158 = ORIENTED_EDGE ( 'NONE', *, *, #15111, .F. ) ;
#4159 = CARTESIAN_POINT ( 'NONE',  ( 0.1167790944451423257, 0.3930555554796889561, -0.2819296736111110424 ) ) ;
#4160 = CARTESIAN_POINT ( 'NONE',  ( 0.000000000000000000, 0.000000000000000000, 0.4425000000000000044 ) ) ;
#4161 = CARTESIAN_POINT ( 'NONE',  ( -0.1236067977499790416, 0.01249999980491520342, 0.3804226065180614236 ) ) ;
#4162 = CARTESIAN_POINT ( 'NONE',  ( 0.4000000000000000222, 0.2571428571428571175, 0.000000000000000000 ) ) ;
#4163 = CARTESIAN_POINT ( 'NONE',  ( 0.2230971623002953874, -0.2230971623002954429, 0.08312500000000162814 ) ) ;
#4164 = CARTESIAN_POINT ( 'NONE',  ( -0.2774186958558242933, -0.3935988683107538577, 0.07439726544913140283 ) ) ;
#4165 = CARTESIAN_POINT ( 'NONE',  ( 5.731347020009612645E-17, 5.009111111111110404, 0.3119999999999999996 ) ) ;
#4166 = CARTESIAN_POINT ( 'NONE',  ( 0.2819296736111110424, 0.5319444443685777957, 0.1167790944451424923 ) ) ;
#4167 = CARTESIAN_POINT ( 'NONE',  ( -0.2819296736111110979, 0.2298611110352444808, -3.452642723725051716E-17 ) ) ;
#4168 = ORIENTED_EDGE ( 'NONE', *, *, #521, .F. ) ;
#4169 = CARTESIAN_POINT ( 'NONE',  ( 0.1167790944451424368, 4.273000000075865223, 0.2819296736111110424 ) ) ;
#4170 = CARTESIAN_POINT ( 'NONE',  ( -0.4000000000000000222, 0.2160714283763437438, 0.1299678784931624920 ) ) ;
#4171 = CARTESIAN_POINT ( 'NONE',  ( 0.1167790944451424368, 4.828555555631421470, 0.2819296736111110424 ) ) ;
#4172 = CARTESIAN_POINT ( 'NONE',  ( -0.1167790944451423119, 4.175777777853643791, -0.2819296736111110979 ) ) ;
#4173 = DIRECTION ( 'NONE',  ( -0.000000000000000000, -1.000000000000000000, -0.000000000000000000 ) ) ;
#4174 = CARTESIAN_POINT ( 'NONE',  ( 0.2209708691207961651, 0.2209708691207959985, 0.09527777777777951540 ) ) ;
#4175 = CARTESIAN_POINT ( 'NONE',  ( 5.731347020009612645E-17, 4.071611111262843252, 0.3119999999999999996 ) ) ;
#4176 = CARTESIAN_POINT ( 'NONE',  ( 0.3119999999999999996, 0.1326388888888885564, -0.1292346314604056468 ) ) ;
#4177 = CARTESIAN_POINT ( 'NONE',  ( -0.1986479633930287036, -0.2391244849435051334, -0.09958585457510185646 ) ) ;
#4178 = ORIENTED_EDGE ( 'NONE', *, *, #19169, .F. ) ;
#4179 = DATE_AND_TIME ( #4299, #1765 ) ;
#4180 = ORIENTED_EDGE ( 'NONE', *, *, #24068, .F. ) ;
#4181 = ORIENTED_EDGE ( 'NONE', *, *, #3813, .F. ) ;
#4182 = CARTESIAN_POINT ( 'NONE',  ( 0.2472135954999579166, 0.3178571428571427826, 0.3402603233408160732 ) ) ;
#4183 = DIRECTION ( 'NONE',  ( -0.000000000000000000, -0.000000000000000000, -1.000000000000000000 ) ) ;
#4184 = CARTESIAN_POINT ( 'NONE',  ( -0.2901050598373867695, 5.005620093107005175, 0.1163399601593286398 ) ) ;
#4185 = EDGE_CURVE ( 'NONE', #14020, #16668, #23768, .T. ) ;
#4186 = ORIENTED_EDGE ( 'NONE', *, *, #20332, .F. ) ;
#4187 = CARTESIAN_POINT ( 'NONE',  ( 0.1292346314604056745, 0.6326388887371557912, -0.3119999999999999996 ) ) ;
#4188 = AXIS2_PLACEMENT_3D ( 'NONE', #7563, #13194, #3906 ) ;
#4189 = ORIENTED_EDGE ( 'NONE', *, *, #666, .F. ) ;
#4190 = CARTESIAN_POINT ( 'NONE',  ( -0.3125000000000000000, 1.913510623667739771E-17, 0.2341666666666698537 ) ) ;
#4191 = CARTESIAN_POINT ( 'NONE',  ( 0.3112631253509388074, 0.3615580281551279418, 0.4252366019055049406 ) ) ;
#4192 = CARTESIAN_POINT ( 'NONE',  ( 0.3613381517857143232, -0.006250000097542392913, 0.000000000000000000 ) ) ;
#4193 = CYLINDRICAL_SURFACE ( 'NONE', #1113, 0.3150000000000000577 ) ;
#4194 = ORIENTED_EDGE ( 'NONE', *, *, #18397, .F. ) ;
#4195 = CARTESIAN_POINT ( 'NONE',  ( 0.2233192592356400275, 0.3080357141881718275, -0.3073725909049499494 ) ) ;
#4196 = DIRECTION ( 'NONE',  ( -0.4999999999999908962, 0.000000000000000000, 0.8660254037844438146 ) ) ;
#4197 = CARTESIAN_POINT ( 'NONE',  ( 0.1144950937579609085, -0.2764156081756484751, 0.4390277777777825130 ) ) ;
#4198 = APPROVAL ( #15023, 'UNKNOWN' ) ;
#4199 = EDGE_CURVE ( 'NONE', #1725, #17904, #5610, .T. ) ;
#4200 = CARTESIAN_POINT ( 'NONE',  ( -0.1167790944451423535, 4.029944444520309865, 0.2819296736111110424 ) ) ;
#4201 = LINE ( 'NONE', #11653, #19195 ) ;
#4202 = CARTESIAN_POINT ( 'NONE',  ( -0.1469396509590103761, 5.191462283868291117, 0.2486211279754877157 ) ) ;
#4203 = CARTESIAN_POINT ( 'NONE',  ( -0.3119999999999999996, 4.776472222373953969, -0.1292346314604056468 ) ) ;
#4204 = CARTESIAN_POINT ( 'NONE',  ( -0.1167790944451423535, 5.043833333409199149, 0.2819296736111110979 ) ) ;
#4205 = VERTEX_POINT ( 'NONE', #16477 ) ;
#4206 = CARTESIAN_POINT ( 'NONE',  ( 0.1167790944451424368, 4.203555555631420582, 0.2819296736111110424 ) ) ;
#4207 = CIRCLE ( 'NONE', #3041, 0.3525000000000007017 ) ;
#4208 = EDGE_LOOP ( 'NONE', ( #19682, #4186, #9707, #18248 ) ) ;
#4209 = CARTESIAN_POINT ( 'NONE',  ( -0.1116596296178199582, 0.1580357141881718608, -0.3436530038418508792 ) ) ;
#4210 = ORIENTED_EDGE ( 'NONE', *, *, #4085, .T. ) ;
#4211 = EDGE_LOOP ( 'NONE', ( #166, #3943 ) ) ;
#4212 = SECURITY_CLASSIFICATION_LEVEL ( 'unclassified' ) ;
#4213 = CARTESIAN_POINT ( 'NONE',  ( 0.3155070326520292290, 0.1306872919485615736, 0.4303472222222270438 ) ) ;
#4214 = CARTESIAN_POINT ( 'NONE',  ( 0.3119999999999999996, 0.2993055555555552139, -0.1292346314604056468 ) ) ;
#4215 = CARTESIAN_POINT ( 'NONE',  ( 0.1993543840281266633, 3.845916666742533074, -0.1993543840281266910 ) ) ;
#4216 =( REPRESENTATION_RELATIONSHIP ('NONE','NONE', #4490, #18521 ) REPRESENTATION_RELATIONSHIP_WITH_TRANSFORMATION ( #1610 )SHAPE_REPRESENTATION_RELATIONSHIP( ) );
#4217 = CARTESIAN_POINT ( 'NONE',  ( 0.1109400265990461154, 4.429522179582135344, -0.2916197229367319954 ) ) ;
#4218 = CARTESIAN_POINT ( 'NONE',  ( 5.731347020009612645E-17, 4.620222222222221120, 0.3119999999999999996 ) ) ;
#4219 = CARTESIAN_POINT ( 'NONE',  ( 0.1590601067977331917, -0.4494324818882468597, 0.07654795713851240968 ) ) ;
#4220 = AXIS2_PLACEMENT_3D ( 'NONE', #5658, #13122, #23813 ) ;
#4221 = CARTESIAN_POINT ( 'NONE',  ( -0.1954553509668046640, 0.1954553509668046918, 0.1925000000000027245 ) ) ;
#4222 = CARTESIAN_POINT ( 'NONE',  ( 0.2819296736111110424, 0.4902777777019112215, 0.1167790944451424923 ) ) ;
#4223 = CARTESIAN_POINT ( 'NONE',  ( -0.2764156081756484196, 1.692557448933383907E-17, -0.1338888888888887796 ) ) ;
#4224 = ORIENTED_EDGE ( 'NONE', *, *, #15315, .T. ) ;
#4225 = CARTESIAN_POINT ( 'NONE',  ( -0.2819296736111110424, 4.648000000075866112, 0.1167790944451424923 ) ) ;
#4226 = CARTESIAN_POINT ( 'NONE',  ( -0.4000000000000000222, 0.4267857140906294311, -4.898587196589413075E-17 ) ) ;
#4227 = EDGE_CURVE ( 'NONE', #21772, #5544, #11108, .T. ) ;
#4228 = CARTESIAN_POINT ( 'NONE',  ( 0.1993543840281267465, 4.651472222298087544, 0.1993543840281266633 ) ) ;
#4229 = CARTESIAN_POINT ( 'NONE',  ( -0.008900482412455170203, 4.155199780624622363, -0.3118911708052335974 ) ) ;
#4230 = CARTESIAN_POINT ( 'NONE',  ( 0.2914760784562323015, 4.866496372597516107, -0.1112933579050594812 ) ) ;
#4231 = CARTESIAN_POINT ( 'NONE',  ( -0.2733612579097375317, -3.892158461848095304E-18, 0.2765269779737352662 ) ) ;
#4232 = DIRECTION ( 'NONE',  ( 0.000000000000000000, 1.000000000000000000, 0.000000000000000000 ) ) ;
#4233 = CARTESIAN_POINT ( 'NONE',  ( -0.2206173157302027676, 4.279944444444443441, 0.2206173157302028787 ) ) ;
#4234 = CARTESIAN_POINT ( 'NONE',  ( -0.1236067977499789583, 0.2785714285714285254, -0.3804226065180614791 ) ) ;
#4235 = CARTESIAN_POINT ( 'NONE',  ( 1.910449006669871087E-17, 0.5249999998482670627, -0.3119999999999999996 ) ) ;
#4236 = ORIENTED_EDGE ( 'NONE', *, *, #13057, .F. ) ;
#4237 = CARTESIAN_POINT ( 'NONE',  ( 0.2729932625349638098, 4.590067353440807629, -0.1570725860997395085 ) ) ;
#4238 = VERTEX_POINT ( 'NONE', #11349 ) ;
#4239 = CARTESIAN_POINT ( 'NONE',  ( 0.2829332492628002238, 4.700467745438439593, -0.1315023910696823672 ) ) ;
#4240 = CIRCLE ( 'NONE', #17874, 0.6211549996190571798 ) ;
#4241 = CARTESIAN_POINT ( 'NONE',  ( 0.3072406530695101501, 4.639533684784892031, 0.05499356144264888613 ) ) ;
#4242 = ADVANCED_FACE ( 'NONE', ( #18539 ), #1952, .F. ) ;
#4243 = CARTESIAN_POINT ( 'NONE',  ( 0.1144950937579611444, 0.2764156081756483641, 0.4598611111111159389 ) ) ;
#4244 = EDGE_CURVE ( 'NONE', #4444, #22975, #2605, .T. ) ;
#4245 = ADVANCED_FACE ( 'NONE', ( #3422 ), #7208, .F. ) ;
#4246 = CARTESIAN_POINT ( 'NONE',  ( 0.2492337893549602668, 4.301904822861448707, 0.1920667163975616487 ) ) ;
#4247 = ORIENTED_EDGE ( 'NONE', *, *, #21838, .F. ) ;
#4248 = CARTESIAN_POINT ( 'NONE',  ( 0.1116596296178199860, -0.06339285724039953052, -0.3436530038418508792 ) ) ;
#4249 = CARTESIAN_POINT ( 'NONE',  ( 0.1167790944451423257, 0.4347222221463555858, -0.2819296736111110424 ) ) ;
#4250 = DIRECTION ( 'NONE',  ( 0.000000000000000000, 0.000000000000000000, -1.000000000000000000 ) ) ;
#4251 = CARTESIAN_POINT ( 'NONE',  ( 0.1920699496354679736, 0.7220375312147633284, -1.080957935066063857 ) ) ;
#4252 = CARTESIAN_POINT ( 'NONE',  ( 0.3125000000000004996, -0.1294417382415918583, 0.08486111111111281635 ) ) ;
#4253 = CARTESIAN_POINT ( 'NONE',  ( -0.2764156081756484196, 1.692557448933383907E-17, 0.1508333333333356785 ) ) ;
#4254 = ADVANCED_FACE ( 'NONE', ( #20372 ), #1829, .T. ) ;
#4255 = CARTESIAN_POINT ( 'NONE',  ( -0.1501324200702761902, 4.622704549112463646, 0.2735036765724895291 ) ) ;
#4256 = DIRECTION ( 'NONE',  ( -0.000000000000000000, -1.000000000000000000, -0.000000000000000000 ) ) ;
#4257 = CARTESIAN_POINT ( 'NONE',  ( -0.2316346313134401980, -9.420544349976220987E-18, -0.3200023620661306412 ) ) ;
#4258 = CARTESIAN_POINT ( 'NONE',  ( 0.1292346314604057023, 0.2298611111111107663, 0.3119999999999998885 ) ) ;
#4259 = CARTESIAN_POINT ( 'NONE',  ( 0.1292346314604056190, 5.144527777777776478, -0.3119999999999999996 ) ) ;
#4260 = CIRCLE ( 'NONE', #14776, 0.3125000000000000000 ) ;
#4261 = CARTESIAN_POINT ( 'NONE',  ( 0.2819296736111110979, 4.116750000075866112, -3.452642723725051716E-17 ) ) ;
#4262 = CARTESIAN_POINT ( 'NONE',  ( -0.2495581641001925477, 4.329761746715313109, -0.1916607439132450852 ) ) ;
#4263 = CARTESIAN_POINT ( 'NONE',  ( -0.1292346314604056190, 0.4729166665149337478, -0.3119999999999999996 ) ) ;
#4264 = DIRECTION ( 'NONE',  ( -0.000000000000000000, 1.000000000000000000, -0.000000000000000000 ) ) ;
#4265 = VERTEX_POINT ( 'NONE', #16714 ) ;
#4266 = ORIENTED_EDGE ( 'NONE', *, *, #18875, .F. ) ;
#4267 = CARTESIAN_POINT ( 'NONE',  ( 0.3124999999999993339, -0.1294417382415928852, 0.1473611111111136351 ) ) ;
#4268 = CARTESIAN_POINT ( 'NONE',  ( -1.726321361862525858E-17, 4.783416666742532186, -0.2819296736111110979 ) ) ;
#4269 = CARTESIAN_POINT ( 'NONE',  ( 0.3613381517857143232, 0.4223214284738860957, 0.000000000000000000 ) ) ;
#4270 = CARTESIAN_POINT ( 'NONE',  ( 0.3854970698558352615, -0.3186990403121960913, 0.4003306813560889577 ) ) ;
#4271 = DIRECTION ( 'NONE',  ( 0.000000000000000000, 0.000000000000000000, 1.000000000000000000 ) ) ;
#4272 = DIRECTION ( 'NONE',  ( 0.000000000000000000, 0.000000000000000000, -1.000000000000000000 ) ) ;
#4273 = CARTESIAN_POINT ( 'NONE',  ( -0.2819296736111110424, 4.259111111186976828, 0.1167790944451424923 ) ) ;
#4274 = COORDINATED_UNIVERSAL_TIME_OFFSET ( 0, 0, .AHEAD. ) ;
#4275 = CARTESIAN_POINT ( 'NONE',  ( -0.01870657908477804665, 4.044342180066220926, -0.3114387789057476708 ) ) ;
#4276 = DIRECTION ( 'NONE',  ( 0.7559289460184540621, 0.6546536707079775308, -0.000000000000000000 ) ) ;
#4277 = CARTESIAN_POINT ( 'NONE',  ( 0.3116633497045768197, 3.673292956572201451, 0.09499999999999995948 ) ) ;
#4278 = CARTESIAN_POINT ( 'NONE',  ( -0.2819296736111110979, 0.4659722221463555303, -3.452642723725051716E-17 ) ) ;
#4279 = CARTESIAN_POINT ( 'NONE',  ( 0.2206173157302027954, 4.141055555555554157, -0.2206173157302028232 ) ) ;
#4280 = CARTESIAN_POINT ( 'NONE',  ( -0.2472135954999579999, 0.3660714283763437105, 0.3402603233408160732 ) ) ;
#4281 = CARTESIAN_POINT ( 'NONE',  ( 0.3236067977499790249, 0.3357142857142856318, -0.2351141009169892826 ) ) ;
#4282 = CARTESIAN_POINT ( 'NONE',  ( 0.000000000000000000, 0.3155070326520292845, 0.2150694444444470887 ) ) ;
#4283 = FACE_OUTER_BOUND ( 'NONE', #1359, .T. ) ;
#4284 = DIRECTION ( 'NONE',  ( 0.000000000000000000, 0.000000000000000000, -1.000000000000000000 ) ) ;
#4285 = CARTESIAN_POINT ( 'NONE',  ( 0.1167790944451423119, 0.5458333332574668573, -0.2819296736111110979 ) ) ;
#4286 = CARTESIAN_POINT ( 'NONE',  ( 1.726321361862525858E-17, 0.2715277777019111660, -0.2819296736111110979 ) ) ;
#4287 = CARTESIAN_POINT ( 'NONE',  ( -0.2819296736111110979, 4.311194444520309865, 0.000000000000000000 ) ) ;
#4288 = CARTESIAN_POINT ( 'NONE',  ( -0.3999999999999999667, 0.2803571426620579676, -0.1299678784931626030 ) ) ;
#4289 = CARTESIAN_POINT ( 'NONE',  ( 0.2819296736111110979, 4.946611111186976828, 0.1167790944451422425 ) ) ;
#4290 = CARTESIAN_POINT ( 'NONE',  ( -0.1993543840281266355, 4.137583333409199149, 0.1993543840281267465 ) ) ;
#4291 = DIRECTION ( 'NONE',  ( 0.000000000000000000, -0.5249267702233982869, 0.8511473937590547933 ) ) ;
#4292 = VECTOR ( 'NONE', #8249, 39.37007874015748143 ) ;
#4293 = ORIENTED_EDGE ( 'NONE', *, *, #16381, .F. ) ;
#4294 = CARTESIAN_POINT ( 'NONE',  ( -0.4749999999999999778, 3.575000000000000622, -0.09499999999999995948 ) ) ;
#4295 = CARTESIAN_POINT ( 'NONE',  ( -0.3119999999999999996, 3.887583333485065573, -0.1292346314604056468 ) ) ;
#4296 = CARTESIAN_POINT ( 'NONE',  ( 0.1064715942167347440, -0.2552471790384449046, 0.3880822748423152224 ) ) ;
#4297 = CARTESIAN_POINT ( 'NONE',  ( 0.4324999999999994404, 2.702499999999999236, -0.01249999999999974742 ) ) ;
#4298 = ORIENTED_EDGE ( 'NONE', *, *, #21779, .F. ) ;
#4299 = CALENDAR_DATE ( 2026, 7, 10 ) ;
#4300 = VECTOR ( 'NONE', #3095, 39.37007874015748854 ) ;
#4301 = CARTESIAN_POINT ( 'NONE',  ( -0.3127083509410205631, 5.002075493856721344, -0.005575882147177812359 ) ) ;
#4302 = EDGE_LOOP ( 'NONE', ( #22602, #14794, #10102, #10681, #2959, #4180 ) ) ;
#4303 = CARTESIAN_POINT ( 'NONE',  ( 0.1167790944451423257, 0.1708333332574666907, -0.2819296736111110424 ) ) ;
#4304 = AXIS2_PLACEMENT_3D ( 'NONE', #2225, #11735, #4039 ) ;
#4305 = EDGE_LOOP ( 'NONE', ( #11897, #7458, #22151, #8038, #14062 ) ) ;
#4306 = CARTESIAN_POINT ( 'NONE',  ( 0.0003767400161662670839, 4.266045432495603862, -0.3119998056229988936 ) ) ;
#4307 = DIRECTION ( 'NONE',  ( -0.000000000000000000, 0.000000000000000000, 1.000000000000000000 ) ) ;
#4308 = DIRECTION ( 'NONE',  ( -0.000000000000000000, -0.000000000000000000, -1.000000000000000000 ) ) ;
#4309 = CARTESIAN_POINT ( 'NONE',  ( -0.1116596296178199582, 0.08660714275960045005, -0.3436530038418508792 ) ) ;
#4310 = CARTESIAN_POINT ( 'NONE',  ( 0.1707342748200432747, 5.171949696446763944, 0.2418557544016106398 ) ) ;
#4311 = EDGE_CURVE ( 'NONE', #1032, #7960, #18223, .T. ) ;
#4312 = EDGE_LOOP ( 'NONE', ( #13864, #136, #23651, #2183, #17958, #11924, #9463, #3827, #10888, #9531, #3058, #21900, #9516, #22950, #4621 ) ) ;
#4313 = CARTESIAN_POINT ( 'NONE',  ( -0.1116596296178199582, 0.3901785713310289561, -0.3436530038418508792 ) ) ;
#4314 = DIRECTION ( 'NONE',  ( 0.4999999999999913403, -0.000000000000000000, 0.8660254037844434816 ) ) ;
#4315 = CARTESIAN_POINT ( 'NONE',  ( -0.2256633871477300712, 4.675584075455893718, 0.2154820786522459730 ) ) ;
#4316 = CARTESIAN_POINT ( 'NONE',  ( 0.1167790944451424368, 4.092444444520309865, 0.2819296736111110424 ) ) ;
#4317 = CARTESIAN_POINT ( 'NONE',  ( -0.4749999999999999778, 3.700000000000000622, -0.09499999999999995948 ) ) ;
#4318 = CARTESIAN_POINT ( 'NONE',  ( -0.2931282487914294022, 5.178805443644709072, -0.02438572332841970960 ) ) ;
#4319 = CARTESIAN_POINT ( 'NONE',  ( -0.2206173157302028232, 4.550777777929510215, -0.2206173157302028232 ) ) ;
#4320 = CARTESIAN_POINT ( 'NONE',  ( -1.726321361862525858E-17, 4.852861111186976828, -0.2819296736111110979 ) ) ;
#4321 = ORIENTED_EDGE ( 'NONE', *, *, #10920, .T. ) ;
#4322 = AXIS2_PLACEMENT_3D ( 'NONE', #18216, #16393, #19675 ) ;
#4323 = CARTESIAN_POINT ( 'NONE',  ( -0.2819296736111110424, 4.356333333409198261, 0.1167790944451424923 ) ) ;
#4324 = EDGE_LOOP ( 'NONE', ( #36, #1115, #5653, #21234 ) ) ;
#4325 = CARTESIAN_POINT ( 'NONE',  ( -0.2923287055106771337, 0.3080357141881718275, -0.2123892367102620804 ) ) ;
#4326 = VERTEX_POINT ( 'NONE', #15014 ) ;
#4327 = ORIENTED_EDGE ( 'NONE', *, *, #11390, .F. ) ;
#4328 = PERSON_AND_ORGANIZATION ( #15518, #2538 ) ;
#4329 = ORIENTED_EDGE ( 'NONE', *, *, #4662, .F. ) ;
#4330 = CC_DESIGN_DATE_AND_TIME_ASSIGNMENT ( #21457, #12091, ( #6872 ) ) ;
#4331 = CARTESIAN_POINT ( 'NONE',  ( -0.2230971623002954152, -0.2230971623002953874, 0.4060416666666712970 ) ) ;
#4332 = DIRECTION ( 'NONE',  ( -0.000000000000000000, -1.000000000000000000, -0.000000000000000000 ) ) ;
#4333 = CARTESIAN_POINT ( 'NONE',  ( 0.1015009281151166981, 3.738732047420452620, -0.2819296736111110979 ) ) ;
#4334 = DIRECTION ( 'NONE',  ( 0.000000000000000000, 0.000000000000000000, -1.000000000000000000 ) ) ;
#4335 = DIRECTION ( 'NONE',  ( -0.000000000000000000, -1.000000000000000000, -0.000000000000000000 ) ) ;
#4336 = CARTESIAN_POINT ( 'NONE',  ( 0.3853527072883956572, -0.3187823880793682063, 0.07808165802388239429 ) ) ;
#4337 = CARTESIAN_POINT ( 'NONE',  ( 0.2764156081756484196, -5.077672346800151106E-17, 0.1716666666666692431 ) ) ;
#4338 = CARTESIAN_POINT ( 'NONE',  ( -0.1167790944451422702, 0.5666666665908000056, -0.2819296736111110979 ) ) ;
#4339 = CARTESIAN_POINT ( 'NONE',  ( -0.1144950937579609779, 0.2764156081756484196, -0.08874999999999953759 ) ) ;
#4340 = EDGE_LOOP ( 'NONE', ( #15670, #16425, #4266, #1598, #3172 ) ) ;
#4341 = CARTESIAN_POINT ( 'NONE',  ( -0.1167790944451423257, 4.634111111186976828, -0.2819296736111110424 ) ) ;
#4342 = CARTESIAN_POINT ( 'NONE',  ( -0.01172578639833055797, -0.5344959914317364280, 0.04874733047934380614 ) ) ;
#4343 = CARTESIAN_POINT ( 'NONE',  ( -0.1167790944451423257, 4.620222222298087544, -0.2819296736111110424 ) ) ;
#4344 = CARTESIAN_POINT ( 'NONE',  ( 0.3119999999999999996, 0.2888888887371559577, 0.000000000000000000 ) ) ;
#4345 = CARTESIAN_POINT ( 'NONE',  ( 0.2810189208971028973, 4.867268483421598901, -0.1357210265892402346 ) ) ;
#4346 = CARTESIAN_POINT ( 'NONE',  ( -0.4749999999999999778, 3.700000000000000622, 0.09499999999999995948 ) ) ;
#4347 = DIRECTION ( 'NONE',  ( 0.4995222938423279913, 0.04370253788966922681, -0.8651979924482608997 ) ) ;
#4348 = CARTESIAN_POINT ( 'NONE',  ( -0.2206173157302028232, 4.266055555555555046, -0.2206173157302028232 ) ) ;
#4349 = CARTESIAN_POINT ( 'NONE',  ( -0.1993543840281266355, 3.859805555631421026, 0.1993543840281267465 ) ) ;
#4350 = SHAPE_REPRESENTATION ( 'Aloris-BXA-Ball', ( #9127 ), #12664 ) ;
#4351 = CARTESIAN_POINT ( 'NONE',  ( -0.3394572874457115752, 3.700000000000000622, 0.09499999999999993172 ) ) ;
#4352 = ORIENTED_EDGE ( 'NONE', *, *, #20196, .F. ) ;
#4353 = DIRECTION ( 'NONE',  ( 0.000000000000000000, 0.000000000000000000, 1.000000000000000000 ) ) ;
#4354 = VERTEX_POINT ( 'NONE', #22436 ) ;
#4355 = ADVANCED_FACE ( 'NONE', ( #5735 ), #9665, .T. ) ;
#4356 = DIRECTION ( 'NONE',  ( 0.000000000000000000, 0.000000000000000000, 1.000000000000000000 ) ) ;
#4357 = DESIGN_CONTEXT ( 'detailed design', #16368, 'design' ) ;
#4358 = ADVANCED_FACE ( 'NONE', ( #2073 ), #13563, .T. ) ;
#4359 = CARTESIAN_POINT ( 'NONE',  ( 0.1913906330737462635, 4.133038910390919973, 0.2464018815271727947 ) ) ;
#4360 = CARTESIAN_POINT ( 'NONE',  ( 0.1954553509668047195, 0.1954553509668046085, 0.4563888888888936735 ) ) ;
#4361 = CARTESIAN_POINT ( 'NONE',  ( -8.379073922441706732E-07, 4.293833316950179224, 0.3119999999988748440 ) ) ;
#4362 = ORIENTED_EDGE ( 'NONE', *, *, #20927, .T. ) ;
#4363 = CARTESIAN_POINT ( 'NONE',  ( -0.1116596296178200276, -0.02767857152611381821, 0.3436530038418508792 ) ) ;
#4364 = CARTESIAN_POINT ( 'NONE',  ( -0.2819296736111110979, 0.5631944443685777957, -3.452642723725051716E-17 ) ) ;
#4365 = CYLINDRICAL_SURFACE ( 'NONE', #16779, 0.3119999999999999996 ) ;
#4366 = CARTESIAN_POINT ( 'NONE',  ( 0.2825688201499270136, 0.3409968823100701374, -1.166126927630756205 ) ) ;
#4367 = DIRECTION ( 'NONE',  ( -0.4995222938423278802, -0.04370253788966928232, 0.8651979924482610107 ) ) ;
#4368 = CARTESIAN_POINT ( 'NONE',  ( -0.2764156081756484196, 1.692557448933383907E-17, 0.2619444444444476994 ) ) ;
#4369 = EDGE_LOOP ( 'NONE', ( #14695, #21279, #17997, #18660 ) ) ;
#4370 = CARTESIAN_POINT ( 'NONE',  ( -0.4749999999999999778, 3.575000000000000622, 0.09499999999999995948 ) ) ;
#4371 = CARTESIAN_POINT ( 'NONE',  ( 0.5097595264191663311, 2.319533376497111554, -0.6691893185836859104 ) ) ;
#4372 = CARTESIAN_POINT ( 'NONE',  ( 0.1272547916512738186, -3.800488706749810574E-17, -0.3527189223800989981 ) ) ;
#4373 = CARTESIAN_POINT ( 'NONE',  ( -0.1292346314604056190, 0.3131944444444441089, -0.3119999999999999996 ) ) ;
#4374 = CARTESIAN_POINT ( 'NONE',  ( 0.3119999999999999996, 4.967444444444443441, -3.820898013339742174E-17 ) ) ;
#4375 = CARTESIAN_POINT ( 'NONE',  ( -0.1167790944451423257, 4.078555555631421470, -0.2819296736111110424 ) ) ;
#4376 = CARTESIAN_POINT ( 'NONE',  ( -0.3119777406883143533, 4.336685373751207884, 0.04102447248701817512 ) ) ;
#4377 = CARTESIAN_POINT ( 'NONE',  ( -0.1568395974156474859, 0.4507144935777588346, 0.4251457422752842330 ) ) ;
#4378 = CARTESIAN_POINT ( 'NONE',  ( 0.3105117338273140071, 4.808796746528941846, -0.03833085760703142109 ) ) ;
#4379 = ORIENTED_EDGE ( 'NONE', *, *, #8802, .F. ) ;
#4380 = EDGE_CURVE ( 'NONE', #1752, #20538, #21338, .T. ) ;
#4381 = VERTEX_POINT ( 'NONE', #15605 ) ;
#4382 = EDGE_CURVE ( 'NONE', #21772, #13133, #11471, .T. ) ;
#4383 = CARTESIAN_POINT ( 'NONE',  ( -3.827021247335479543E-17, -0.3125000000000000000, 0.1369444444444468667 ) ) ;
#4384 = CARTESIAN_POINT ( 'NONE',  ( 0.2819296736111110424, 4.717444444520309865, -0.1167790944451423396 ) ) ;
#4385 = FACE_OUTER_BOUND ( 'NONE', #9237, .T. ) ;
#4386 = CARTESIAN_POINT ( 'NONE',  ( 0.1956796206285028594, -0.4282901957204846011, 0.4181140142936810578 ) ) ;
#4387 = ADVANCED_FACE ( 'NONE', ( #9637 ), #16947, .T. ) ;
#4388 = PERSON_AND_ORGANIZATION ( #15518, #2538 ) ;
#4389 = CARTESIAN_POINT ( 'NONE',  ( -0.4687500000000003331, 0.04364354118082217765, 0.07944686358224754830 ) ) ;
#4390 = LINE ( 'NONE', #4150, #13435 ) ;
#4391 = CARTESIAN_POINT ( 'NONE',  ( -0.2819296736111110979, 4.418833333409199149, -0.1167790944451422980 ) ) ;
#4392 = CARTESIAN_POINT ( 'NONE',  ( -0.3077216217399622589, 4.056174970759743204, -0.05514810450480703979 ) ) ;
#4393 = CARTESIAN_POINT ( 'NONE',  ( -0.2764156081756484196, 1.692557448933383907E-17, -0.01583333333333230425 ) ) ;
#4394 = CARTESIAN_POINT ( 'NONE',  ( -0.2209708691207961373, -0.2209708691207961095, 0.3522222222222263222 ) ) ;
#4395 = EDGE_LOOP ( 'NONE', ( #21377, #1328, #4004, #7021, #8656, #12424 ) ) ;
#4396 = CARTESIAN_POINT ( 'NONE',  ( -5.178964085587577574E-17, 0.3687499999241333204, 0.2819296736111110979 ) ) ;
#4397 = DIRECTION ( 'NONE',  ( 0.4999999999999912292, 0.000000000000000000, -0.8660254037844437036 ) ) ;
#4398 = CARTESIAN_POINT ( 'NONE',  ( -0.3236067977499790249, 0.1571428571428570564, 0.2351141009169892271 ) ) ;
#4399 = LINE ( 'NONE', #11861, #8394 ) ;
#4400 = CARTESIAN_POINT ( 'NONE',  ( -0.2230971623002954152, -0.2230971623002953874, 0.2359027777777805979 ) ) ;
#4401 = VECTOR ( 'NONE', #10688, 39.37007874015748143 ) ;
#4402 = CARTESIAN_POINT ( 'NONE',  ( 0.000000000000000000, 3.700000000000000622, 0.000000000000000000 ) ) ;
#4403 = CARTESIAN_POINT ( 'NONE',  ( -7.892860322346445127E-13, 5.206640035683665957, 0.2819296736111106538 ) ) ;
#4404 = CARTESIAN_POINT ( 'NONE',  ( 1.726321361862525858E-17, 0.4937499999241333759, -0.2819296736111110979 ) ) ;
#4405 = CARTESIAN_POINT ( 'NONE',  ( -5.178964085587577574E-17, 0.1881944443685778512, 0.2819296736111110979 ) ) ;
#4406 = ORIENTED_EDGE ( 'NONE', *, *, #14382, .T. ) ;
#4407 = CARTESIAN_POINT ( 'NONE',  ( 0.2819296736111110424, 4.175777777853643791, -0.1167790944451423396 ) ) ;
#4408 = CARTESIAN_POINT ( 'NONE',  ( 0.2472135954999579166, 0.3803571426620580564, 0.3402603233408160732 ) ) ;
#4409 = CARTESIAN_POINT ( 'NONE',  ( 0.2819296736111110979, 4.783416666742532186, -3.452642723725051716E-17 ) ) ;
#4410 = EDGE_CURVE ( 'NONE', #16571, #20545, #8035, .T. ) ;
#4411 = CARTESIAN_POINT ( 'NONE',  ( 0.3089396748338966714, 5.077109074767299113, 0.05201469694613055500 ) ) ;
#4412 = EDGE_CURVE ( 'NONE', #14624, #10770, #6879, .T. ) ;
#4413 = ORIENTED_EDGE ( 'NONE', *, *, #15590, .T. ) ;
#4414 = CARTESIAN_POINT ( 'NONE',  ( 0.3124999999999993339, 0.1294417382415928297, 0.09180555555555727776 ) ) ;
#4415 = CARTESIAN_POINT ( 'NONE',  ( -0.2206173157302028232, 3.828555555707287894, -0.2206173157302028232 ) ) ;
#4416 = DIRECTION ( 'NONE',  ( -0.000000000000000000, -1.000000000000000000, -0.000000000000000000 ) ) ;
#4417 = ADVANCED_FACE ( 'NONE', ( #603 ), #19254, .T. ) ;
#4418 = EDGE_LOOP ( 'NONE', ( #22676, #17249, #6262, #14209 ) ) ;
#4419 = PERSON_AND_ORGANIZATION_ROLE ( 'creator' ) ;
#4420 = ORIENTED_EDGE ( 'NONE', *, *, #14991, .F. ) ;
#4421 = CARTESIAN_POINT ( 'NONE',  ( 0.2784250239278243666, 0.03789337644375263825, 0.3924996019884888221 ) ) ;
#4422 = CARTESIAN_POINT ( 'NONE',  ( -0.03922383558181956331, 5.014860061204379882, 0.3120000079912765845 ) ) ;
#4423 = ORIENTED_EDGE ( 'NONE', *, *, #14087, .T. ) ;
#4424 = CARTESIAN_POINT ( 'NONE',  ( 0.1167790944451423535, 0.1499999999241333759, 0.2819296736111110424 ) ) ;
#4425 = CARTESIAN_POINT ( 'NONE',  ( 0.2723612931040907958, 4.247528608451006882, 0.1575966107290118767 ) ) ;
#4426 = CARTESIAN_POINT ( 'NONE',  ( 0.000000000000000000, 0.06786299768266475241, 0.000000000000000000 ) ) ;
#4427 = CARTESIAN_POINT ( 'NONE',  ( 4.898587196589413075E-17, 3.700000000000000622, 0.4000000000000000222 ) ) ;
#4428 = CARTESIAN_POINT ( 'NONE',  ( -0.1116596296178200276, 0.2580357141881718941, 0.3436530038418508792 ) ) ;
#4429 = CARTESIAN_POINT ( 'NONE',  ( 0.3950000000000000178, 2.665000000000000036, -0.2605837454876624437 ) ) ;
#4430 = ORIENTED_EDGE ( 'NONE', *, *, #620, .T. ) ;
#4431 = CARTESIAN_POINT ( 'NONE',  ( 0.3613381517857143232, 0.2937499999024575370, 0.1174058825155741975 ) ) ;
#4432 = CARTESIAN_POINT ( 'NONE',  ( -0.3885631146789287338, -0.3299392016703766028, 0.06110928887248354840 ) ) ;
#4433 = AXIS2_PLACEMENT_3D ( 'NONE', #20154, #6990, #21620 ) ;
#4434 = CARTESIAN_POINT ( 'NONE',  ( -0.2819296736111110979, 4.075083333409199149, 0.000000000000000000 ) ) ;
#4435 = CARTESIAN_POINT ( 'NONE',  ( 0.07786113151988235948, 5.041682425470480844, -0.3026906604598632033 ) ) ;
#4436 = CARTESIAN_POINT ( 'NONE',  ( -0.2638604546507810622, 5.184694301399809468, 0.1249839293704117366 ) ) ;
#4437 = CARTESIAN_POINT ( 'NONE',  ( -0.3119999999999999996, 4.502166666818398610, 0.000000000000000000 ) ) ;
#4438 = CARTESIAN_POINT ( 'NONE',  ( 0.2819296736111111534, 4.835500000075866112, 0.1167790944451422563 ) ) ;
#4439 = EDGE_LOOP ( 'NONE', ( #15957, #13604, #16612, #461 ) ) ;
#4440 = CARTESIAN_POINT ( 'NONE',  ( -0.2819296736111110424, 3.967444444520310309, 0.1167790944451424923 ) ) ;
#4441 = ORIENTED_EDGE ( 'NONE', *, *, #15409, .F. ) ;
#4442 = CARTESIAN_POINT ( 'NONE',  ( -0.1116596296178200276, 0.2580357141881718941, 0.3436530038418508792 ) ) ;
#4443 = EDGE_CURVE ( 'NONE', #18346, #4780, #10829, .T. ) ;
#4444 = VERTEX_POINT ( 'NONE', #2559 ) ;
#4445 = B_SPLINE_CURVE_WITH_KNOTS ( 'NONE', 3,
 ( #21985, #21502, #5156, #12747, #4919, #6873, #20162, #3450, #21749, #10656 ),
 .UNSPECIFIED., .F., .F.,
 ( 4, 2, 2, 2, 4 ),
 ( 0.000000000000000000, 0.003321891969150509404, 0.006643783938301018807, 0.009965675907451529078, 0.01328756787660204108 ),
 .UNSPECIFIED. ) ;
#4446 = ORIENTED_EDGE ( 'NONE', *, *, #22382, .F. ) ;
#4447 = PERSON_AND_ORGANIZATION ( #15518, #2538 ) ;
#4448 = AXIS2_PLACEMENT_3D ( 'NONE', #6000, #11267, #515 ) ;
#4449 = ORIENTED_EDGE ( 'NONE', *, *, #23504, .T. ) ;
#4450 = FACE_OUTER_BOUND ( 'NONE', #1373, .T. ) ;
#4451 = DIRECTION ( 'NONE',  ( 0.000000000000000000, 1.000000000000000000, 0.000000000000000000 ) ) ;
#4452 = CARTESIAN_POINT ( 'NONE',  ( -0.3119999999999999996, 0.1534722220704892726, 0.1292346314604056190 ) ) ;
#4453 = CARTESIAN_POINT ( 'NONE',  ( 0.1764925855509518193, 5.136404133670642302, 0.2495434643755579940 ) ) ;
#4454 = CARTESIAN_POINT ( 'NONE',  ( -0.4687500000000003886, -0.02223792287132515463, 0.4181395016878637905 ) ) ;
#4455 = CARTESIAN_POINT ( 'NONE',  ( 0.1294417382415924134, 0.3124999999999999445, 0.2723611111111146621 ) ) ;
#4456 = CARTESIAN_POINT ( 'NONE',  ( 0.1650087075157316563, -0.4586159948670568420, 0.07156199457778184003 ) ) ;
#4457 = CARTESIAN_POINT ( 'NONE',  ( -0.1954553509668046918, -0.1954553509668046640, 0.2063888888888917028 ) ) ;
#4458 = CARTESIAN_POINT ( 'NONE',  ( -0.2819296736111111534, 0.1222222221463555719, 0.1167790944451422563 ) ) ;
#4459 = CARTESIAN_POINT ( 'NONE',  ( -0.1954553509668046918, -0.1954553509668046640, 0.3800000000000041678 ) ) ;
#4460 = VERTEX_POINT ( 'NONE', #20847 ) ;
#4461 = CARTESIAN_POINT ( 'NONE',  ( 0.2819296736111110424, 4.675777777853643791, -0.1167790944451423396 ) ) ;
#4462 = CARTESIAN_POINT ( 'NONE',  ( 4.898587196589413075E-17, 3.700000000000000622, 0.4000000000000000222 ) ) ;
#4463 = CARTESIAN_POINT ( 'NONE',  ( 0.2819296736111110979, 4.599388888964753619, 0.1167790944451422425 ) ) ;
#4464 = CARTESIAN_POINT ( 'NONE',  ( -0.0006352866450341495630, 4.154962694833915116, -0.3119993937163639264 ) ) ;
#4465 = CARTESIAN_POINT ( 'NONE',  ( 0.3080281032009763997, 4.865139504843591034, -0.06764252334466071270 ) ) ;
#4466 = CYLINDRICAL_SURFACE ( 'NONE', #15669, 0.3125000000000000000 ) ;
#4467 = FACE_BOUND ( 'NONE', #22915, .T. ) ;
#4468 = CARTESIAN_POINT ( 'NONE',  ( -0.3119999999999999996, 4.272999999999998799, 0.000000000000000000 ) ) ;
#4469 = CARTESIAN_POINT ( 'NONE',  ( -0.3616234456863465230, 3.514980167629567998, 2.635972749958888528 ) ) ;
#4470 = VECTOR ( 'NONE', #21337, 39.37007874015748143 ) ;
#4471 = CARTESIAN_POINT ( 'NONE',  ( 0.06396586966202466584, 4.962292326657688157, 0.3053748286811586166 ) ) ;
#4472 = CC_DESIGN_PERSON_AND_ORGANIZATION_ASSIGNMENT ( #10076, #15905, ( #14409 ) ) ;
#4473 = ORIENTED_EDGE ( 'NONE', *, *, #6647, .T. ) ;
#4474 = FACE_OUTER_BOUND ( 'NONE', #7093, .T. ) ;
#4475 = EDGE_LOOP ( 'NONE', ( #22864, #15264, #2600, #6507, #10436, #10846 ) ) ;
#4476 = LOCAL_TIME ( 21, 9, 13.00000000000000000, #9349 ) ;
#4477 = CARTESIAN_POINT ( 'NONE',  ( 0.01791502114354955391, 4.710015879029342045, -0.3115078771295382576 ) ) ;
#4478 = CARTESIAN_POINT ( 'NONE',  ( 0.1918308770790998485, 4.133054567813140068, 0.2460591670449067125 ) ) ;
#4479 = CARTESIAN_POINT ( 'NONE',  ( -0.3155070326520293400, 0.1306872919485614903, 0.06229166666666853536 ) ) ;
#4480 = AXIS2_PLACEMENT_3D ( 'NONE', #2188, #7664, #465 ) ;
#4481 = CARTESIAN_POINT ( 'NONE',  ( -0.004466634099735791383, 3.932848888112731700, -0.3119725945497263675 ) ) ;
#4482 = ADVANCED_FACE ( 'NONE', ( #13310 ), #723, .F. ) ;
#4483 = CARTESIAN_POINT ( 'NONE',  ( -0.2923287055106771337, 0.09374999990245758141, -0.2123892367102620804 ) ) ;
#4484 = CARTESIAN_POINT ( 'NONE',  ( 0.2819296736111110424, 0.4763888888130222710, 0.1167790944451424923 ) ) ;
#4485 = FACE_OUTER_BOUND ( 'NONE', #10551, .T. ) ;
#4486 = CARTESIAN_POINT ( 'NONE',  ( 0.3613381517857143232, 0.01160714275960046671, 0.000000000000000000 ) ) ;
#4487 = DIRECTION ( 'NONE',  ( 0.8660254037844389297, -0.4999999999999995559, 0.000000000000000000 ) ) ;
#4488 = DIRECTION ( 'NONE',  ( 0.000000000000000000, 0.000000000000000000, 1.000000000000000000 ) ) ;
#4489 = ORIENTED_EDGE ( 'NONE', *, *, #14723, .T. ) ;
#4490 = SHAPE_REPRESENTATION ( 'MAS-409', ( #9551, #958, #10310, #16539, #6002, #19639, #4834, #13840, #23538, #13069 ), #16549 ) ;
#4491 = LINE ( 'NONE', #837, #16901 ) ;
#4492 = LINE ( 'NONE', #9876, #22974 ) ;
#4493 = PRODUCT_DEFINITION_FORMATION_WITH_SPECIFIED_SOURCE ( 'ANY', '', #7006, .NOT_KNOWN. ) ;
#4494 = CARTESIAN_POINT ( 'NONE',  ( 0.2206173157302027954, 4.752166666666665762, -0.2206173157302028232 ) ) ;
#4495 = CARTESIAN_POINT ( 'NONE',  ( -0.3119999999999999996, 0.5423611111111107386, -0.1292346314604056745 ) ) ;
#4496 = CARTESIAN_POINT ( 'NONE',  ( 0.3119999999999999996, 4.963972222222222008, 0.1292346314604056190 ) ) ;
#4497 = CC_DESIGN_PERSON_AND_ORGANIZATION_ASSIGNMENT ( #15645, #2717, ( #16981 ) ) ;
#4498 = CARTESIAN_POINT ( 'NONE',  ( -0.1993543840281266355, 3.873694444520310309, 0.1993543840281267465 ) ) ;
#4499 = CARTESIAN_POINT ( 'NONE',  ( -0.3119999999999998885, 3.832027777777776922, 0.1292346314604058410 ) ) ;
#4500 = CARTESIAN_POINT ( 'NONE',  ( -0.04612934949349477981, 0.5146330850176630278, 0.3902021065398098565 ) ) ;
#4501 = CARTESIAN_POINT ( 'NONE',  ( 0.000000000000000000, 2.662805069640206135, -0.8823420915204682746 ) ) ;
#4502 = ORIENTED_EDGE ( 'NONE', *, *, #14381, .T. ) ;
#4503 = EDGE_LOOP ( 'NONE', ( #13855, #19529, #22628, #10807 ) ) ;
#4504 = CARTESIAN_POINT ( 'NONE',  ( -0.2494960723420805160, 4.008026183271772958, 0.1917385534842481476 ) ) ;
#4505 = CARTESIAN_POINT ( 'NONE',  ( -0.1993543840281266355, 4.748694444520309865, 0.1993543840281267465 ) ) ;
#4506 = VECTOR ( 'NONE', #21405, 39.37007874015748143 ) ;
#4507 = CARTESIAN_POINT ( 'NONE',  ( -0.03928873229836517267, 5.166389717777303936, 0.2957448058751782627 ) ) ;
#4508 = PERSON_AND_ORGANIZATION ( #15518, #2538 ) ;
#4509 = CARTESIAN_POINT ( 'NONE',  ( -0.2977100099089716734, 3.575000000000000622, 0.09499999999999993172 ) ) ;
#4510 = DIRECTION ( 'NONE',  ( -0.000000000000000000, -1.000000000000000000, -0.000000000000000000 ) ) ;
#4511 = LOCAL_TIME ( 21, 9, 13.00000000000000000, #11883 ) ;
#4512 = CARTESIAN_POINT ( 'NONE',  ( 0.2819296736111110979, 4.227861111186976828, -3.452642723725051716E-17 ) ) ;
#4513 = CARTESIAN_POINT ( 'NONE',  ( -0.1292346314604105872, 4.873694444444444329, -0.3119999999999950591 ) ) ;
#4514 = CARTESIAN_POINT ( 'NONE',  ( -0.2764156081756484196, -0.1144950937579609362, 0.1543055555555579716 ) ) ;
#4515 = CARTESIAN_POINT ( 'NONE',  ( 0.000000000000000000, 5.384999999999999787, 0.000000000000000000 ) ) ;
#4516 = ORIENTED_EDGE ( 'NONE', *, *, #369, .F. ) ;
#4517 = VECTOR ( 'NONE', #21844, 39.37007874015748143 ) ;
#4518 = CARTESIAN_POINT ( 'NONE',  ( -0.1993543840281266633, 0.5145833332574667462, -0.1993543840281266910 ) ) ;
#4519 = CARTESIAN_POINT ( 'NONE',  ( 0.4796768774581259831, 0.08621990061574087705, 0.07157892306036504892 ) ) ;
#4520 = EDGE_CURVE ( 'NONE', #11205, #23206, #6006, .T. ) ;
#4521 = CARTESIAN_POINT ( 'NONE',  ( 1.658214884748263618, 0.000000000000000000, -2.174029041877829638 ) ) ;
#4522 = CIRCLE ( 'NONE', #1787, 0.3125000000000000000 ) ;
#4523 = CARTESIAN_POINT ( 'NONE',  ( -0.3999999999999999667, 0.3607142857142855430, -0.1299678784931626030 ) ) ;
#4524 = CARTESIAN_POINT ( 'NONE',  ( 0.1306872919485616846, 0.3155070326520292290, 0.2671527777777808477 ) ) ;
#4525 = EDGE_LOOP ( 'NONE', ( #7726, #6936, #17713, #19332, #19944 ) ) ;
#4526 = DIRECTION ( 'NONE',  ( 0.000000000000000000, -0.7071067811865475727, -0.7071067811865475727 ) ) ;
#4527 = CARTESIAN_POINT ( 'NONE',  ( 1.106602540378444965, 0.000000000000000000, -2.540999999999999925 ) ) ;
#4528 = CARTESIAN_POINT ( 'NONE',  ( -0.2819296736111110979, 0.4486111110352445364, -0.1167790944451423396 ) ) ;
#4529 = CARTESIAN_POINT ( 'NONE',  ( -0.1167790944451424368, 0.2958333332574667462, 0.2819296736111110424 ) ) ;
#4530 = CARTESIAN_POINT ( 'NONE',  ( -0.1167790944451423257, 3.967444444520310309, -0.2819296736111110424 ) ) ;
#4531 = CARTESIAN_POINT ( 'NONE',  ( 0.3999999999999999667, 0.2517857140906293867, -0.1299678784931625475 ) ) ;
#4532 = EDGE_CURVE ( 'NONE', #9492, #2739, #15077, .T. ) ;
#4533 = CARTESIAN_POINT ( 'NONE',  ( -0.1993543840281266355, 4.540361111186976828, 0.1993543840281267465 ) ) ;
#4534 = CARTESIAN_POINT ( 'NONE',  ( 0.2690855894900002210, 5.073817426067109615, 0.1585580871995575791 ) ) ;
#4535 = EDGE_LOOP ( 'NONE', ( #14464, #1404, #12647, #15872 ) ) ;
#4536 = VERTEX_POINT ( 'NONE', #19025 ) ;
#4537 = DIRECTION ( 'NONE',  ( 0.000000000000000000, 0.000000000000000000, -1.000000000000000000 ) ) ;
#4538 = CARTESIAN_POINT ( 'NONE',  ( 0.1292346314604058410, 3.852861111262843696, 0.3119999999999998885 ) ) ;
#4539 = CARTESIAN_POINT ( 'NONE',  ( 0.1961415469428243463, -0.1956144934195144791, 0.3880822748423151114 ) ) ;
#4540 = VECTOR ( 'NONE', #12371, 39.37007874015748854 ) ;
#4541 = ORIENTED_EDGE ( 'NONE', *, *, #9010, .T. ) ;
#4542 = PERSON_AND_ORGANIZATION_ROLE ( 'creator' ) ;
#4543 = CARTESIAN_POINT ( 'NONE',  ( 0.2107751267066954592, 0.1916353986792963815, 0.3959111835198027007 ) ) ;
#4544 = ADVANCED_FACE ( 'NONE', ( #7802 ), #5964, .T. ) ;
#4545 = CARTESIAN_POINT ( 'NONE',  ( -0.2902335162209870867, 4.998847991299789406, -0.1145027670670989706 ) ) ;
#4546 = ORIENTED_EDGE ( 'NONE', *, *, #9191, .F. ) ;
#4547 = CARTESIAN_POINT ( 'NONE',  ( -0.1993543840281267465, 0.08402777770191115214, 0.1993543840281266633 ) ) ;
#4548 = ADVANCED_FACE ( 'NONE', ( #12204 ), #10365, .T. ) ;
#4549 = ORIENTED_EDGE ( 'NONE', *, *, #9313, .T. ) ;
#4550 = CARTESIAN_POINT ( 'NONE',  ( -0.1236067977499790416, 0.02142857142857140795, 0.3804226065180614236 ) ) ;
#4551 = CARTESIAN_POINT ( 'NONE',  ( -0.2832489717015474473, 4.728264267671256960, 0.1346859133935131569 ) ) ;
#4552 = CARTESIAN_POINT ( 'NONE',  ( -4.684274006738626122E-17, 1.530000000000000027, 0.000000000000000000 ) ) ;
#4553 = CARTESIAN_POINT ( 'NONE',  ( -0.2923287055106771337, 0.2508928570453147211, 0.2123892367102619971 ) ) ;
#4554 = DIRECTION ( 'NONE',  ( -1.177540334020096294E-17, 0.2588190451025213501, -0.9659258262890682012 ) ) ;
#4555 = B_SPLINE_CURVE_WITH_KNOTS ( 'NONE', 3,
 ( #3404, #9015, #16457, #23869, #5350, #12817, #20234, #3525, #10976, #18401, #13408, #20710, #17415, #22661, #11947, #19121, #19362, #19010, #2305, #8136, #22777, #22542, #4481, #9990, #9498, #17294, #6189, #9620, #9743, #15469 ),
 .UNSPECIFIED., .F., .F.,
 ( 4, 2, 2, 2, 2, 2, 2, 2, 2, 2, 1, 1, 1, 1, 1, 1, 2, 4 ),
 ( 0.8315072053056934420, 0.8337924113469056264, 0.8360776173881179218, 0.8383628234293301063, 0.8406480294705422907, 0.8429332355117545861, 0.8452184415529667705, 0.8475036475941790659, 0.8486462506147851581, 0.8492175521250882042, 0.8495032028802397273, 0.8496460282578154333, 0.8497174409466033973, 0.8497531472909972683, 0.8497710004631943148, 0.8497799270492927270, 0.8497843903423419887, 0.8497888536353912503 ),
 .UNSPECIFIED. ) ;
#4556 = CARTESIAN_POINT ( 'NONE',  ( -0.3613381517857143232, 0.3330357141881718497, -4.425116109941954795E-17 ) ) ;
#4557 = CARTESIAN_POINT ( 'NONE',  ( 1.573500000000000343, 2.683750000000000746, -1.818749999999999645 ) ) ;
#4558 = ORIENTED_EDGE ( 'NONE', *, *, #4078, .F. ) ;
#4559 = EDGE_CURVE ( 'NONE', #13125, #17792, #2269, .T. ) ;
#4560 = CARTESIAN_POINT ( 'NONE',  ( 5.178964085587577574E-17, 3.811194444520309865, 0.2819296736111110979 ) ) ;
#4561 = CARTESIAN_POINT ( 'NONE',  ( -0.3119999999999999996, 0.09097222207048930032, -0.1292346314604056745 ) ) ;
#4562 = CARTESIAN_POINT ( 'NONE',  ( 5.731347020009612645E-17, 4.342444444444443441, 0.3119999999999999996 ) ) ;
#4563 = LINE ( 'NONE', #12022, #5805 ) ;
#4564 = CARTESIAN_POINT ( 'NONE',  ( 0.3119999999999999996, 4.470916666818398610, 0.1292346314604056190 ) ) ;
#4565 = CARTESIAN_POINT ( 'NONE',  ( 0.2819296736111111534, 4.668833333409200037, 0.1167790944451422563 ) ) ;
#4566 = ORIENTED_EDGE ( 'NONE', *, *, #1736, .T. ) ;
#4567 = CARTESIAN_POINT ( 'NONE',  ( -0.1993543840281266355, 4.082027777853643791, 0.1993543840281267465 ) ) ;
#4568 = ADVANCED_FACE ( 'NONE', ( #955 ), #15723, .T. ) ;
#4569 = EDGE_LOOP ( 'NONE', ( #17878, #9998, #8657, #1820 ) ) ;
#4570 = EDGE_CURVE ( 'NONE', #9859, #1154, #23136, .T. ) ;
#4571 = AXIS2_PLACEMENT_3D ( 'NONE', #833, #6317, #2893 ) ;
#4572 = ORIENTED_EDGE ( 'NONE', *, *, #6592, .F. ) ;
#4573 = PERSON_AND_ORGANIZATION ( #15518, #2538 ) ;
#4574 = ORIENTED_EDGE ( 'NONE', *, *, #20332, .T. ) ;
#4575 = CARTESIAN_POINT ( 'NONE',  ( 0.4805070082343982918, 0.2560807851245620048, 0.04413116910602137705 ) ) ;
#4576 = LINE ( 'NONE', #17269, #6941 ) ;
#4577 = ORIENTED_EDGE ( 'NONE', *, *, #7239, .F. ) ;
#4578 = CARTESIAN_POINT ( 'NONE',  ( 0.2206173157302028232, 0.01805555540382262902, -0.2206173157302028232 ) ) ;
#4579 = FACE_OUTER_BOUND ( 'NONE', #1706, .T. ) ;
#4580 = CARTESIAN_POINT ( 'NONE',  ( -0.4687500000000003886, 0.1752294869986955883, 0.4001773373238182718 ) ) ;
#4581 = CARTESIAN_POINT ( 'NONE',  ( 0.2209708691207961651, 0.2209708691207959985, 0.2688888888888923412 ) ) ;
#4582 = DIRECTION ( 'NONE',  ( -0.000000000000000000, -0.9961946980917454342, 0.08715574274765830465 ) ) ;
#4583 = CARTESIAN_POINT ( 'NONE',  ( 0.1993543840281266355, 0.08402777770191115214, 0.1993543840281267465 ) ) ;
#4584 = CARTESIAN_POINT ( 'NONE',  ( -0.2764156081756484196, 0.1144950937579609918, 0.1404166666666689656 ) ) ;
#4585 = EDGE_LOOP ( 'NONE', ( #22779, #13479, #12087, #3462 ) ) ;
#4586 = DIRECTION ( 'NONE',  ( 0.000000000000000000, -0.000000000000000000, 1.000000000000000000 ) ) ;
#4587 = EDGE_CURVE ( 'NONE', #12971, #7634, #22825, .T. ) ;
#4588 = CARTESIAN_POINT ( 'NONE',  ( -0.1167790944451423535, 4.585500000075865223, 0.2819296736111110424 ) ) ;
#4589 = CARTESIAN_POINT ( 'NONE',  ( 3.827021247335478926E-17, 3.700000000000000622, 0.3125000000000000000 ) ) ;
#4590 = CARTESIAN_POINT ( 'NONE',  ( -0.1302323571378496414, 0.2053342067589494779, -1.229370332884858863 ) ) ;
#4591 = DIRECTION ( 'NONE',  ( -1.000000000000000000, 0.000000000000000000, 0.000000000000000000 ) ) ;
#4592 = CARTESIAN_POINT ( 'NONE',  ( 0.4875000000000002665, -0.2598076211353317899, 0.06112444011295373181 ) ) ;
#4593 = CARTESIAN_POINT ( 'NONE',  ( -0.3119999999999999996, 4.325083333333331836, -0.1292346314604056468 ) ) ;
#4594 = AXIS2_PLACEMENT_3D ( 'NONE', #9883, #13553, #8152 ) ;
#4595 = CARTESIAN_POINT ( 'NONE',  ( 0.3119999999999999996, 5.193138889040620043, 0.1292346314604056190 ) ) ;
#4596 = CARTESIAN_POINT ( 'NONE',  ( 0.3112369449188003290, 4.973790024703991897, 0.02198042532292469528 ) ) ;
#4597 = CARTESIAN_POINT ( 'NONE',  ( -0.5116234456863466562, 0.9548081934128183068, 2.549370209580444246 ) ) ;
#4598 = CARTESIAN_POINT ( 'NONE',  ( 0.3101174172661914086, 0.3622195030262473359, 0.08858683671056809261 ) ) ;
#4599 = VERTEX_POINT ( 'NONE', #21562 ) ;
#4600 = CARTESIAN_POINT ( 'NONE',  ( 0.1294417382415921358, -0.3125000000000002220, 0.08486111111111313554 ) ) ;
#4601 = DESIGN_CONTEXT ( 'detailed design', #12648, 'design' ) ;
#4602 = FACE_OUTER_BOUND ( 'NONE', #7366, .T. ) ;
#4603 = CARTESIAN_POINT ( 'NONE',  ( 0.1306872919485614071, -0.3155070326520293955, 0.08312500000000203060 ) ) ;
#4604 = CARTESIAN_POINT ( 'NONE',  ( -0.3119999999999999996, 4.439666666666665762, 0.000000000000000000 ) ) ;
#4605 = CARTESIAN_POINT ( 'NONE',  ( 2.326421213736078119E-17, 0.2973214284738861513, -0.3799334167787516425 ) ) ;
#4606 = CARTESIAN_POINT ( 'NONE',  ( -0.2819296736111110979, 0.07708333325746669074, -3.452642723725051716E-17 ) ) ;
#4607 = CARTESIAN_POINT ( 'NONE',  ( 0.2764156081756484196, -5.077672346800151106E-17, 0.1230555555555576941 ) ) ;
#4608 = CARTESIAN_POINT ( 'NONE',  ( 0.2527126213444991776, -0.1892291168970930137, 0.4228708124548452574 ) ) ;
#4609 = DIRECTION ( 'NONE',  ( -1.000000000000000000, 0.000000000000000000, 6.148297094540788948E-16 ) ) ;
#4610 = CARTESIAN_POINT ( 'NONE',  ( -0.1954553509668046918, -0.1954553509668046640, 0.3800000000000041678 ) ) ;
#4611 = ORIENTED_EDGE ( 'NONE', *, *, #8462, .F. ) ;
#4612 = CARTESIAN_POINT ( 'NONE',  ( -0.1432526013158665901, 4.622930756421714804, 0.2772325657423325707 ) ) ;
#4613 = CARTESIAN_POINT ( 'NONE',  ( -0.1785261131399872025, 4.288481118505546696, 0.2582360697992498455 ) ) ;
#4614 = LINE ( 'NONE', #476, #8256 ) ;
#4615 = CARTESIAN_POINT ( 'NONE',  ( 1.910449006669871087E-17, 0.3652777777777774237, -0.3119999999999999996 ) ) ;
#4616 = CARTESIAN_POINT ( 'NONE',  ( -0.3119999999999999996, 5.050777777777776478, 0.000000000000000000 ) ) ;
#4617 = CARTESIAN_POINT ( 'NONE',  ( 0.2819296736111110424, 4.064666666742532186, -0.1167790944451423396 ) ) ;
#4618 = DIRECTION ( 'NONE',  ( 0.4999999999999916178, 0.000000000000000000, 0.8660254037844433705 ) ) ;
#4619 = FACE_OUTER_BOUND ( 'NONE', #4208, .T. ) ;
#4620 = CARTESIAN_POINT ( 'NONE',  ( 0.000000000000000000, 0.1199999999999999956, 0.000000000000000000 ) ) ;
#4621 = ORIENTED_EDGE ( 'NONE', *, *, #15666, .F. ) ;
#4622 = ORIENTED_EDGE ( 'NONE', *, *, #16678, .F. ) ;
#4623 = CYLINDRICAL_SURFACE ( 'NONE', #13248, 0.3119999999999999996 ) ;
#4624 = CARTESIAN_POINT ( 'NONE',  ( -0.2819296736111110424, 4.627166666742532186, -0.1167790944451423119 ) ) ;
#4625 = CARTESIAN_POINT ( 'NONE',  ( 1.995346317926969793E-07, 4.516063323326865664, 0.3119999999998666063 ) ) ;
#4626 = PERSON_AND_ORGANIZATION ( #15518, #2538 ) ;
#4627 = CARTESIAN_POINT ( 'NONE',  ( -0.4796773749965631550, -0.08638149583431357914, 0.07156438896664418792 ) ) ;
#4628 = CARTESIAN_POINT ( 'NONE',  ( 0.1954553509668046640, -0.1954553509668047195, -0.001944444444443294917 ) ) ;
#4629 = CARTESIAN_POINT ( 'NONE',  ( 0.1993543840281266633, 4.012583333409199149, -0.1993543840281266910 ) ) ;
#4630 = CALENDAR_DATE ( 2026, 7, 10 ) ;
#4631 = DIRECTION ( 'NONE',  ( 0.8660254037844434816, -0.000000000000000000, -0.4999999999999913403 ) ) ;
#4632 = CARTESIAN_POINT ( 'NONE',  ( 0.03162548898803060199, 5.072453936747297831, 0.3108465394227510337 ) ) ;
#4633 =( BOUNDED_CURVE ( )  B_SPLINE_CURVE ( 2, ( #22557, #483, #19027, #20968, #9514, #22675, #9397, #5849, #22313, #16948, #5611, #11596, #247 ),
 .UNSPECIFIED., .F., .T. ) 
 B_SPLINE_CURVE_WITH_KNOTS ( ( 3, 2, 2, 2, 2, 2, 3 ),
 ( 0.8214285714285715079, 0.8285714285714286254, 0.8428571428571428603, 0.8571428571428570953, 0.8714285714285714413, 0.8857142857142856762, 0.8928571428571429047 ),
 .UNSPECIFIED. ) 
 CURVE ( )  GEOMETRIC_REPRESENTATION_ITEM ( )  RATIONAL_B_SPLINE_CURVE ( ( 0.9755282581475768211, 0.9755282581475769321, 1.000000000000000000, 0.9510565162951535312, 1.000000000000000000, 0.9510565162951535312, 1.000000000000000000, 0.9510565162951535312, 1.000000000000000000, 0.9510565162951535312, 1.000000000000000000, 0.9755282581475765991, 0.9755282581475768211 ) ) 
 REPRESENTATION_ITEM ( '' )  );
#4634 = CARTESIAN_POINT ( 'NONE',  ( 0.000000000000000000, 0.2764156081756484196, 0.1925000000000026690 ) ) ;
#4635 =( BOUNDED_SURFACE ( )  B_SPLINE_SURFACE ( 3, 2, ( 
 ( #19539, #2831, #1008 ),
 ( #16608, #8926, #3552 ),
 ( #14902, #11003, #11122 ),
 ( #18431, #5505, #5624 ),
 ( #14668, #21964, #18670 ),
 ( #13206, #1726, #16726 ) ),
 .UNSPECIFIED., .F., .F., .F. ) 
 B_SPLINE_SURFACE_WITH_KNOTS ( ( 4, 2, 4 ),
 ( 3, 3 ),
 ( 0.001022076388580720786, 0.001521441877679463508, 0.002020807366778206229 ),
 ( 0.000000000000000000, 1.000000000000000000 ),
 .UNSPECIFIED. ) 
 GEOMETRIC_REPRESENTATION_ITEM ( )  RATIONAL_B_SPLINE_SURFACE ( (
 ( 1.000000000000000000, 0.8285407536241355952, 1.000000000000000000),
 ( 1.000000000000000000, 0.8382697314793432497, 1.000000000000000000),
 ( 1.000000000000000000, 0.8433836253082970247, 1.000000000000000000),
 ( 1.000000000000000000, 0.8433992480895827759, 1.000000000000000000),
 ( 1.000000000000000000, 0.8382827608168984534, 1.000000000000000000),
 ( 1.000000000000000000, 0.8285407536241036208, 1.000000000000000000) ) ) 
 REPRESENTATION_ITEM ( '' )  SURFACE ( )  );
#4636 = CARTESIAN_POINT ( 'NONE',  ( 0.3236067977499789694, 0.2499999999999999167, 0.2351141009169893659 ) ) ;
#4637 = VECTOR ( 'NONE', #16566, 39.37007874015748143 ) ;
#4638 = CARTESIAN_POINT ( 'NONE',  ( 1.726321361862525858E-17, 0.1048611110352444808, -0.2819296736111110979 ) ) ;
#4639 = LINE ( 'NONE', #12105, #14292 ) ;
#4640 = LINE ( 'NONE', #15860, #4687 ) ;
#4641 = FACE_OUTER_BOUND ( 'NONE', #159, .T. ) ;
#4642 = CARTESIAN_POINT ( 'NONE',  ( -0.2230971623002953874, 0.2230971623002954152, 0.3886805555555595815 ) ) ;
#4643 = CARTESIAN_POINT ( 'NONE',  ( -0.3125000000000010547, 0.1294417382415911921, 0.05708333333333479032 ) ) ;
#4644 = CARTESIAN_POINT ( 'NONE',  ( -1.853979398150703436E-06, 4.543833384706993606, -0.3119999999944916280 ) ) ;
#4645 = CARTESIAN_POINT ( 'NONE',  ( -0.2819296736111110979, 0.3965277777019111660, -3.452642723725051716E-17 ) ) ;
#4646 = CARTESIAN_POINT ( 'NONE',  ( 0.1167790944451423257, 0.5458333332574666352, -0.2819296736111110424 ) ) ;
#4647 = CARTESIAN_POINT ( 'NONE',  ( -0.2819296736111110424, 4.085500000075865223, -0.1167790944451423119 ) ) ;
#4648 = CARTESIAN_POINT ( 'NONE',  ( -0.3613381517857144343, 0.1223214284738861624, 0.1174058825155740171 ) ) ;
#4649 = CARTESIAN_POINT ( 'NONE',  ( 0.1167790944451424368, 4.661888888964754507, 0.2819296736111110424 ) ) ;
#4650 = DIRECTION ( 'NONE',  ( -0.5000000000000037748, 0.000000000000000000, -0.8660254037844362651 ) ) ;
#4651 = CARTESIAN_POINT ( 'NONE',  ( 0.2896569607109293898, 5.081861310233479756, -0.1164848292807667690 ) ) ;
#4652 = ORIENTED_EDGE ( 'NONE', *, *, #11311, .F. ) ;
#4653 = CARTESIAN_POINT ( 'NONE',  ( 1.573500000000000343, 0.02500000000000021302, -0.1650000000000001465 ) ) ;
#4654 = CARTESIAN_POINT ( 'NONE',  ( -0.2206173157302028232, 3.773000000151732092, -0.2206173157302028232 ) ) ;
#4655 = ADVANCED_FACE ( 'NONE', ( #1326 ), #8513, .T. ) ;
#4656 = DIRECTION ( 'NONE',  ( 1.000000000000000000, 0.000000000000000000, 0.000000000000000000 ) ) ;
#4657 = VECTOR ( 'NONE', #19383, 39.37007874015748143 ) ;
#4658 = EDGE_CURVE ( 'NONE', #19257, #18090, #6566, .T. ) ;
#4659 = CARTESIAN_POINT ( 'NONE',  ( 0.2610103255563372415, 0.03242967361111056407, 0.1075682626660545288 ) ) ;
#4660 = PERSON_AND_ORGANIZATION ( #15518, #2538 ) ;
#4661 = VERTEX_POINT ( 'NONE', #6687 ) ;
#4662 = EDGE_CURVE ( 'NONE', #3037, #23444, #14132, .T. ) ;
#4663 = FACE_OUTER_BOUND ( 'NONE', #7853, .T. ) ;
#4664 = CARTESIAN_POINT ( 'NONE',  ( -0.01780398822517776855, 4.571142336066150946, 0.3116242173092940715 ) ) ;
#4665 = ORIENTED_EDGE ( 'NONE', *, *, #2764, .T. ) ;
#4666 = CARTESIAN_POINT ( 'NONE',  ( -0.2819296736111110979, 0.1326388888130222710, -3.452642723725051716E-17 ) ) ;
#4667 = ORIENTED_EDGE ( 'NONE', *, *, #6146, .T. ) ;
#4668 = CARTESIAN_POINT ( 'NONE',  ( 0.2819296736111110979, -0.006250000075866630166, 0.000000000000000000 ) ) ;
#4669 = CARTESIAN_POINT ( 'NONE',  ( -0.1761266028516242366, 4.732970605661459551, 0.2598151860325674800 ) ) ;
#4670 = DIRECTION ( 'NONE',  ( -9.239214857301838159E-19, -0.9961946980917454342, 0.08715574274765830465 ) ) ;
#4671 = CARTESIAN_POINT ( 'NONE',  ( -0.3613381517857143232, 0.2437499999024575481, -4.425116109941954795E-17 ) ) ;
#4672 = CARTESIAN_POINT ( 'NONE',  ( -0.02115692209977381583, 5.070961635096757014, 0.3120000024408280948 ) ) ;
#4673 = VECTOR ( 'NONE', #10384, 39.37007874015748854 ) ;
#4674 = CARTESIAN_POINT ( 'NONE',  ( 0.2235833740012116433, -0.1735833740012113768, -0.4097528311786164390 ) ) ;
#4675 = VECTOR ( 'NONE', #16181, 39.37007874015748143 ) ;
#4676 = CARTESIAN_POINT ( 'NONE',  ( -0.2890877230579003143, 4.665425013968962809, -0.1173655244367800971 ) ) ;
#4677 = CARTESIAN_POINT ( 'NONE',  ( -0.1993543840281266910, 5.248694444520310753, -0.1993543840281266910 ) ) ;
#4678 = CARTESIAN_POINT ( 'NONE',  ( -0.1292346314604056190, 0.08402777762604483891, -0.3119999999999999996 ) ) ;
#4679 = CARTESIAN_POINT ( 'NONE',  ( -0.2631359636943425562, 5.174404950919535118, -0.1348571213356563603 ) ) ;
#4680 = CARTESIAN_POINT ( 'NONE',  ( -0.3102357779240257352, 4.778494202458470674, -0.05181659030984726161 ) ) ;
#4681 = CARTESIAN_POINT ( 'NONE',  ( -0.3119999999999998885, 4.616750000151732536, 0.1292346314604058410 ) ) ;
#4682 = CARTESIAN_POINT ( 'NONE',  ( 5.178964085587577574E-17, 4.658416666742532186, 0.2819296736111110979 ) ) ;
#4683 = ORIENTED_EDGE ( 'NONE', *, *, #7642, .F. ) ;
#4684 = CARTESIAN_POINT ( 'NONE',  ( 0.1993543840281266633, 3.998694444520309865, -0.1993543840281266910 ) ) ;
#4685 = ADVANCED_FACE ( 'NONE', ( #12320 ), #8751, .T. ) ;
#4686 = VECTOR ( 'NONE', #3753, 39.37007874015748854 ) ;
#4687 = VECTOR ( 'NONE', #6468, 39.37007874015748143 ) ;
#4688 = PERSON_AND_ORGANIZATION ( #15518, #2538 ) ;
#4689 = EDGE_CURVE ( 'NONE', #6065, #1879, #23621, .T. ) ;
#4690 = DIRECTION ( 'NONE',  ( 0.8233282866803208755, -0.5459676143495163503, -0.1550802902806971972 ) ) ;
#4691 = CARTESIAN_POINT ( 'NONE',  ( -0.3125000000000000000, 1.913510623667739771E-17, 0.2272222222222250176 ) ) ;
#4692 = CARTESIAN_POINT ( 'NONE',  ( 0.1292346314604056745, 0.07708333318160039138, -0.3119999999999999996 ) ) ;
#4693 = DIRECTION ( 'NONE',  ( 0.4985709748471340297, 0.07555085810113193467, 0.8635502596144368770 ) ) ;
#4694 = CARTESIAN_POINT ( 'NONE',  ( 0.1292346314604056745, 0.1881944442927115102, -0.3119999999999999996 ) ) ;
#4695 = CARTESIAN_POINT ( 'NONE',  ( 0.7188945565055682163, 2.836044817640776206, -0.6580815178912685637 ) ) ;
#4696 = VERTEX_POINT ( 'NONE', #10482 ) ;
#4697 = CARTESIAN_POINT ( 'NONE',  ( 0.1954553509668046640, -0.1954553509668047195, 0.3869444444444487541 ) ) ;
#4698 = CARTESIAN_POINT ( 'NONE',  ( 0.2819296736111110979, 0.1465277777019111383, 0.000000000000000000 ) ) ;
#4699 = CARTESIAN_POINT ( 'NONE',  ( -0.2764156081756484196, 0.1144950937579609918, 0.02930555555555695163 ) ) ;
#4700 = LINE ( 'NONE', #4462, #17111 ) ;
#4701 = CARTESIAN_POINT ( 'NONE',  ( 0.2819296736111110979, 4.547305555631421470, -3.452642723725051716E-17 ) ) ;
#4702 = CARTESIAN_POINT ( 'NONE',  ( 0.2573004767273346927, 0.1442547113246375190, -0.08399358639954626615 ) ) ;
#4703 = DIRECTION ( 'NONE',  ( 0.000000000000000000, 0.2773500981126160725, -0.9607689228305223983 ) ) ;
#4704 = CARTESIAN_POINT ( 'NONE',  ( 1.573500000000000343, -3.414809992080329023E-17, -0.5649999999999999467 ) ) ;
#4705 = CARTESIAN_POINT ( 'NONE',  ( 0.2206173157302028232, 0.4624999998482670627, -0.2206173157302028232 ) ) ;
#4706 = CARTESIAN_POINT ( 'NONE',  ( -0.3119999999999998885, 4.387583333333331836, 0.1292346314604058410 ) ) ;
#4707 = CIRCLE ( 'NONE', #17961, 0.01874999999999997502 ) ;
#4708 = CARTESIAN_POINT ( 'NONE',  ( -0.2206173157302027676, 5.175777777929509327, 0.2206173157302028787 ) ) ;
#4709 = CARTESIAN_POINT ( 'NONE',  ( 5.731347020009612645E-17, 4.675777777777777366, 0.3119999999999999996 ) ) ;
#4710 = CARTESIAN_POINT ( 'NONE',  ( 0.4620259694561525410, 0.2880908832651559726, 0.04413116910601652676 ) ) ;
#4711 = ORIENTED_EDGE ( 'NONE', *, *, #2280, .F. ) ;
#4712 = CARTESIAN_POINT ( 'NONE',  ( 0.000000000000000000, 5.579732050807569621, 0.000000000000000000 ) ) ;
#4713 = CARTESIAN_POINT ( 'NONE',  ( -0.6211549996190571798, 0.000000000000000000, -0.1199999999999999956 ) ) ;
#4714 = CARTESIAN_POINT ( 'NONE',  ( 0.4692113125120487838, -0.2611562006105975775, 0.04763592618478877661 ) ) ;
#4715 = CARTESIAN_POINT ( 'NONE',  ( 0.1306872919485614071, -0.3155070326520293955, 0.02756944444444603404 ) ) ;
#4716 = CARTESIAN_POINT ( 'NONE',  ( 0.1961921601747127764, 0.4279942808755098915, 0.09139393128962811086 ) ) ;
#4717 = CARTESIAN_POINT ( 'NONE',  ( 0.3119999807920359469, 3.806624880628000085, 0.04084226214478610395 ) ) ;
#4718 = CARTESIAN_POINT ( 'NONE',  ( -0.1116596296178200276, 0.3294642856167432354, 0.3436530038418508792 ) ) ;
#4719 = CARTESIAN_POINT ( 'NONE',  ( 0.2819296736111110424, 0.04583333325746670461, 0.1167790944451424923 ) ) ;
#4720 = CARTESIAN_POINT ( 'NONE',  ( -0.1954553509668046918, -0.1954553509668046640, -0.008888888888887799475 ) ) ;
#4721 = CARTESIAN_POINT ( 'NONE',  ( 0.4449999999999992850, 0.000000000000000000, -0.4000000000000000222 ) ) ;
#4722 = CARTESIAN_POINT ( 'NONE',  ( 0.1294417382415921358, -0.3125000000000002220, 0.07791666666666827168 ) ) ;
#4723 = CARTESIAN_POINT ( 'NONE',  ( -0.2764156081756484196, 1.692557448933383907E-17, 0.3730555555555596925 ) ) ;
#4724 = EDGE_LOOP ( 'NONE', ( #14736, #22960, #21011, #14180 ) ) ;
#4725 = DIRECTION ( 'NONE',  ( -0.000000000000000000, -1.000000000000000000, -0.000000000000000000 ) ) ;
#4726 = CARTESIAN_POINT ( 'NONE',  ( -0.1736506380193462984, 4.271243467713559561, -0.2598347738710399257 ) ) ;
#4727 = DIRECTION ( 'NONE',  ( -0.000000000000000000, -1.000000000000000000, -0.000000000000000000 ) ) ;
#4728 = CARTESIAN_POINT ( 'NONE',  ( -0.1292346314604058410, 0.3895833333333328929, 0.3119999999999998885 ) ) ;
#4729 = CARTESIAN_POINT ( 'NONE',  ( 0.3119999999999999996, 5.022999999999999687, -3.820898013339742174E-17 ) ) ;
#4730 = CARTESIAN_POINT ( 'NONE',  ( -0.2819296736111110979, 4.186194444520309865, 0.000000000000000000 ) ) ;
#4731 = CARTESIAN_POINT ( 'NONE',  ( 0.2819296736111110424, 4.009111111186976828, -0.1167790944451423396 ) ) ;
#4732 = DIRECTION ( 'NONE',  ( 1.000000000000000000, 0.000000000000000000, 0.000000000000000000 ) ) ;
#4733 = FACE_OUTER_BOUND ( 'NONE', #21508, .T. ) ;
#4734 = ORIENTED_EDGE ( 'NONE', *, *, #11843, .F. ) ;
#4735 = ORIENTED_EDGE ( 'NONE', *, *, #9191, .T. ) ;
#4736 = CARTESIAN_POINT ( 'NONE',  ( 0.1294417382415924134, 0.3124999999999999445, 0.1056944444444466308 ) ) ;
#4737 = CARTESIAN_POINT ( 'NONE',  ( -0.1993543840281266355, 4.415361111186976828, 0.1993543840281267465 ) ) ;
#4738 = CARTESIAN_POINT ( 'NONE',  ( -0.1987419572019689940, 5.161870250129094728, 0.2237073997642387846 ) ) ;
#4739 = EDGE_CURVE ( 'NONE', #13614, #20425, #14016, .T. ) ;
#4740 = COORDINATED_UNIVERSAL_TIME_OFFSET ( 0, 0, .AHEAD. ) ;
#4741 = CARTESIAN_POINT ( 'NONE',  ( 0.03762146087705321024, 0.5076544266709851483, 0.4065068718547070747 ) ) ;
#4742 = CARTESIAN_POINT ( 'NONE',  ( -0.2764156081756484196, 1.692557448933383907E-17, -0.07833333333333278303 ) ) ;
#4743 = ADVANCED_BREP_SHAPE_REPRESENTATION ( '', ( #1044, #9127 ), #5239 ) ;
#4744 = CARTESIAN_POINT ( 'NONE',  ( 0.2819296736111110979, 4.175777777853643791, -0.1167790944451423396 ) ) ;
#4745 = CARTESIAN_POINT ( 'NONE',  ( -0.3125412538830298903, 4.835929051231298459, 0.01504738431389416112 ) ) ;
#4746 = CARTESIAN_POINT ( 'NONE',  ( -0.3125000000000000000, 1.913510623667739771E-17, 0.2827777777777810142 ) ) ;
#4747 = CARTESIAN_POINT ( 'NONE',  ( -0.1954553509668046640, 0.1954553509668046918, 0.1994444444444471720 ) ) ;
#4748 = CARTESIAN_POINT ( 'NONE',  ( 0.3613381517857143232, 0.07946428561674329094, 0.1174058825155742114 ) ) ;
#4749 = CARTESIAN_POINT ( 'NONE',  ( 0.1167790944451423535, 0.1361111110352444808, 0.2819296736111110424 ) ) ;
#4750 = CARTESIAN_POINT ( 'NONE',  ( -0.2663714005177904576, 0.1275804160634904094, 0.4068622647240436319 ) ) ;
#4751 = DIRECTION ( 'NONE',  ( -0.000000000000000000, -0.000000000000000000, 1.000000000000000000 ) ) ;
#4752 = CARTESIAN_POINT ( 'NONE',  ( -0.1236067977499789583, 0.1357142857142856485, -0.3804226065180614791 ) ) ;
#4753 = CARTESIAN_POINT ( 'NONE',  ( 0.000000000000000000, 5.500232050807569273, -0.3125000000000001665 ) ) ;
#4754 = CARTESIAN_POINT ( 'NONE',  ( -0.1306872919485615459, -0.3155070326520293400, 0.2949305555555589153 ) ) ;
#4755 = CARTESIAN_POINT ( 'NONE',  ( 0.2206173157302028787, 3.960499999999999243, 0.2206173157302027954 ) ) ;
#4756 = CARTESIAN_POINT ( 'NONE',  ( -0.3125000000000000000, 1.913510623667739771E-17, 0.3938888888888930628 ) ) ;
#4757 = DIRECTION ( 'NONE',  ( -0.000000000000000000, -1.000000000000000000, -0.000000000000000000 ) ) ;
#4758 = CARTESIAN_POINT ( 'NONE',  ( 0.2819296736111110979, 0.4798611110352444808, 0.000000000000000000 ) ) ;
#4759 = CARTESIAN_POINT ( 'NONE',  ( -0.1993543840281266355, 4.151472222298088433, 0.1993543840281267465 ) ) ;
#4760 = CARTESIAN_POINT ( 'NONE',  ( -0.2923287055106771337, -0.03125000009754238389, -0.2123892367102620804 ) ) ;
#4761 = VERTEX_POINT ( 'NONE', #23496 ) ;
#4762 = CONICAL_SURFACE ( 'NONE', #3602, 0.2124999999999999944, 0.7853981633974463916 ) ;
#4763 = CARTESIAN_POINT ( 'NONE',  ( 0.2819296736111110424, 4.620222222298088433, -0.1167790944451423396 ) ) ;
#4764 = CARTESIAN_POINT ( 'NONE',  ( 0.2439254949411622519, 5.136159674610036419, -0.1850816115523053751 ) ) ;
#4765 = CARTESIAN_POINT ( 'NONE',  ( -5.731347020009612645E-17, 0.3861111109593781676, 0.3119999999999999996 ) ) ;
#4766 = ORIENTED_EDGE ( 'NONE', *, *, #1482, .F. ) ;
#4767 = CARTESIAN_POINT ( 'NONE',  ( 0.6396424860381280109, 7.834898727884920884E-17, -0.01143517789850382292 ) ) ;
#4768 = CARTESIAN_POINT ( 'NONE',  ( 0.2206173157302027954, 3.814666666818399055, -0.2206173157302028232 ) ) ;
#4769 = APPROVAL ( #2396, 'UNSPECIFIED' ) ;
#4770 = DIRECTION ( 'NONE',  ( 0.000000000000000000, 0.000000000000000000, 1.000000000000000000 ) ) ;
#4771 =( BOUNDED_CURVE ( )  B_SPLINE_CURVE ( 2, ( #754, #23055, #13810, #8788, #23769, #9036, #9274, #1358, #21835 ),
 .UNSPECIFIED., .F., .F. ) 
 B_SPLINE_CURVE_WITH_KNOTS ( ( 3, 2, 2, 2, 3 ),
 ( 0.1875000000000000000, 0.1979166666666666574, 0.2083333333333333426, 0.2187500000000000000, 0.2291666666666666574 ),
 .UNSPECIFIED. ) 
 CURVE ( )  GEOMETRIC_REPRESENTATION_ITEM ( )  RATIONAL_B_SPLINE_CURVE ( ( 1.000000000000000000, 0.9238795325112867385, 1.000000000000000000, 0.9238795325112867385, 1.000000000000000000, 0.9238795325112867385, 1.000000000000000000, 0.9238795325112867385, 1.000000000000000000 ) ) 
 REPRESENTATION_ITEM ( '' )  );
#4772 = ORIENTED_EDGE ( 'NONE', *, *, #20735, .T. ) ;
#4773 =( BOUNDED_CURVE ( )  B_SPLINE_CURVE ( 2, ( #1391, #16269, #14445, #15784, #12626, #3099, #17979, #14076, #21630, #4795, #20043, #14196, #1149 ),
 .UNSPECIFIED., .F., .T. ) 
 B_SPLINE_CURVE_WITH_KNOTS ( ( 3, 2, 2, 2, 2, 2, 3 ),
 ( 0.4642857142857143016, 0.4714285714285714191, 0.4857142857142857095, 0.5000000000000000000, 0.5142857142857142350, 0.5285714285714285809, 0.5357142857142856984 ),
 .UNSPECIFIED. ) 
 CURVE ( )  GEOMETRIC_REPRESENTATION_ITEM ( )  RATIONAL_B_SPLINE_CURVE ( ( 0.9755282581475767101, 0.9755282581475768211, 1.000000000000000000, 0.9510565162951535312, 1.000000000000000000, 0.9510565162951535312, 1.000000000000000000, 0.9510565162951535312, 1.000000000000000000, 0.9510565162951535312, 1.000000000000000000, 0.9755282581475768211, 0.9755282581475768211 ) ) 
 REPRESENTATION_ITEM ( '' )  );
#4774 = CARTESIAN_POINT ( 'NONE',  ( 5.178964085587577574E-17, 4.811194444520309865, 0.2819296736111110979 ) ) ;
#4775 = DATE_TIME_ROLE ( 'creation_date' ) ;
#4776 = ORIENTED_EDGE ( 'NONE', *, *, #16978, .F. ) ;
#4777 = VECTOR ( 'NONE', #14074, 39.37007874015748143 ) ;
#4778 = CARTESIAN_POINT ( 'NONE',  ( -0.3072307265066616666, 5.116075199176159494, 0.03881433307613120498 ) ) ;
#4779 = CARTESIAN_POINT ( 'NONE',  ( 0.3119999999999999996, 0.2402777777777774515, 0.000000000000000000 ) ) ;
#4780 = VERTEX_POINT ( 'NONE', #6811 ) ;
#4781 = CARTESIAN_POINT ( 'NONE',  ( 0.1167790944451423535, 0.3722222221463555858, 0.2819296736111110424 ) ) ;
#4782 = CARTESIAN_POINT ( 'NONE',  ( 0.1167790944451423257, 0.1152777777019111521, -0.2819296736111110424 ) ) ;
#4783 = DIRECTION ( 'NONE',  ( -0.4999999999999990008, 0.8660254037844391517, -9.106159978880873451E-16 ) ) ;
#4784 = CARTESIAN_POINT ( 'NONE',  ( 0.1971363941232131822, 4.093330204894787272, -0.2454781584649298742 ) ) ;
#4785 = CARTESIAN_POINT ( 'NONE',  ( -0.1116596296178199582, 0.3008928570453147100, -0.3436530038418508792 ) ) ;
#4786 = LINE ( 'NONE', #5146, #10466 ) ;
#4787 = CARTESIAN_POINT ( 'NONE',  ( 0.01848103877824613592, -0.5441716683897390716, 0.04413116910601658227 ) ) ;
#4788 = DIMENSIONAL_EXPONENTS ( 1.000000000000000000, 0.000000000000000000, 0.000000000000000000, 0.000000000000000000, 0.000000000000000000, 0.000000000000000000, 0.000000000000000000 ) ;
#4789 = CARTESIAN_POINT ( 'NONE',  ( -0.2884725026384663549, 4.665377838955494738, -0.1188664842351418310 ) ) ;
#4790 = CARTESIAN_POINT ( 'NONE',  ( -1.726321361862525858E-17, 3.838972222298087544, -0.2819296736111110979 ) ) ;
#4791 = CARTESIAN_POINT ( 'NONE',  ( -0.4366234456863467006, 0.9548081934128058723, 2.592671479769666387 ) ) ;
#4792 = CARTESIAN_POINT ( 'NONE',  ( 0.3125000000000000000, -5.740531871003217465E-17, 0.3730555555555599145 ) ) ;
#4793 = B_SPLINE_CURVE_WITH_KNOTS ( 'NONE', 3,
 ( #8922, #20616, #3916, #7216, #14930, #517, #9802, #22711, #13233, #11510, #13115, #13468, #9675, #11753, #16752, #20885, #17112, #158, #11386, #3826, #18818, #21004, #22835, #2112, #5771, #9553, #7482, #22349, #4177, #7953, #7718, #20531, #15052, #18945 ),
 .UNSPECIFIED., .F., .F.,
 ( 4, 2, 2, 2, 2, 2, 2, 2, 2, 2, 2, 2, 2, 2, 2, 2, 4 ),
 ( 0.02754951627422265806, 0.02882399678900620515, 0.03009847730378974878, 0.03137295781857329935, 0.03264743833335684298, 0.03392191884814039354, 0.03519639936292394411, 0.03647087987770748774, 0.03774536039249104524, 0.03901984090727458887, 0.04029432142205813944, 0.04156880193684169000, 0.04284328245162523363, 0.04411776296640878420, 0.04539224348119233476, 0.04666672399597587839, 0.04794120451075942896 ),
 .UNSPECIFIED. ) ;
#4794 = CARTESIAN_POINT ( 'NONE',  ( 0.1839153728783990138, 0.05322839143466908535, 0.2408560696376421950 ) ) ;
#4795 = CARTESIAN_POINT ( 'NONE',  ( -0.2472135954999579999, 0.2232142855192008613, 0.3402603233408160732 ) ) ;
#4796 = CARTESIAN_POINT ( 'NONE',  ( -0.3119999999999999996, 4.613277777929510215, 0.000000000000000000 ) ) ;
#4797 = CIRCLE ( 'NONE', #18430, 0.01874999999999999237 ) ;
#4798 = EDGE_CURVE ( 'NONE', #175, #16785, #21737, .T. ) ;
#4799 = CARTESIAN_POINT ( 'NONE',  ( 0.2819296736111110979, 4.731333333409200925, -0.1167790944451423396 ) ) ;
#4800 = CARTESIAN_POINT ( 'NONE',  ( 0.2819296736111110979, 4.154944444520309865, 0.1167790944451422425 ) ) ;
#4801 = ORIENTED_EDGE ( 'NONE', *, *, #2887, .T. ) ;
#4802 = EDGE_LOOP ( 'NONE', ( #3922, #9926, #16449, #9587 ) ) ;
#4803 = APPROVAL_ROLE ( '' ) ;
#4804 = ORIENTED_EDGE ( 'NONE', *, *, #20816, .T. ) ;
#4805 = CARTESIAN_POINT ( 'NONE',  ( 1.573500000000000343, 0.000000000000000000, -1.412500000000000089 ) ) ;
#4806 = CARTESIAN_POINT ( 'NONE',  ( 0.000000000000000000, 0.000000000000000000, 0.000000000000000000 ) ) ;
#4807 = CARTESIAN_POINT ( 'NONE',  ( 0.3119999999999999996, 0.07013888873715595773, -0.1292346314604056468 ) ) ;
#4808 = DIRECTION ( 'NONE',  ( -0.4999999999999918954, -0.000000000000000000, -0.8660254037844431485 ) ) ;
#4809 = AXIS2_PLACEMENT_3D ( 'NONE', #19279, #8298, #6471 ) ;
#4810 = CARTESIAN_POINT ( 'NONE',  ( -0.4687500000000003886, -0.1119141212732240320, 0.4216323756266210920 ) ) ;
#4811 = CARTESIAN_POINT ( 'NONE',  ( 0.7847114317029997288, 2.978485840173427324, -0.8855837454876586134 ) ) ;
#4812 = ORIENTED_EDGE ( 'NONE', *, *, #8726, .F. ) ;
#4813 = DIRECTION ( 'NONE',  ( 0.000000000000000000, 0.000000000000000000, -1.000000000000000000 ) ) ;
#4814 = PLANE ( 'NONE',  #15587 ) ;
#4815 = CARTESIAN_POINT ( 'NONE',  ( -0.1144950937579609779, 0.2764156081756484196, 0.1334722222222244348 ) ) ;
#4816 = CARTESIAN_POINT ( 'NONE',  ( -1.726321361862525858E-17, 4.394527777853643791, -0.2819296736111110979 ) ) ;
#4817 = DIRECTION ( 'NONE',  ( 0.000000000000000000, 0.000000000000000000, -1.000000000000000000 ) ) ;
#4818 = CARTESIAN_POINT ( 'NONE',  ( -0.07172508667748003774, 0.7801245175820353817, -1.079864711465235327 ) ) ;
#4819 = CARTESIAN_POINT ( 'NONE',  ( -7.000945310522701902E-17, 0.3821428571428570620, 0.3999999999999999667 ) ) ;
#4820 = CARTESIAN_POINT ( 'NONE',  ( 0.1292346314604056745, 0.4659722220704892726, -0.3119999999999999996 ) ) ;
#4821 = CARTESIAN_POINT ( 'NONE',  ( -0.2206173157302028232, 4.099388888888888083, -0.2206173157302028232 ) ) ;
#4822 = CARTESIAN_POINT ( 'NONE',  ( -1.910449006669871087E-17, 5.210500000151731648, -0.3119999999999999996 ) ) ;
#4823 = ADVANCED_FACE ( 'NONE', ( #3151 ), #17670, .F. ) ;
#4824 = CARTESIAN_POINT ( 'NONE',  ( 0.06147612581608680876, 4.962219778033143847, 0.3058837411390394889 ) ) ;
#4825 = VERTEX_POINT ( 'NONE', #18029 ) ;
#4826 = LINE ( 'NONE', #19710, #5836 ) ;
#4827 = ORIENTED_EDGE ( 'NONE', *, *, #5893, .F. ) ;
#4828 = AXIS2_PLACEMENT_3D ( 'NONE', #13707, #2712, #12126 ) ;
#4829 = CARTESIAN_POINT ( 'NONE',  ( -0.5116234456863258950, 3.706421428007538488, -2.785118725032278419 ) ) ;
#4830 = CARTESIAN_POINT ( 'NONE',  ( -0.1338087529395441955, -0.2734308413694009343, 0.4156188565751802733 ) ) ;
#4831 = EDGE_CURVE ( 'NONE', #13516, #22476, #18632, .T. ) ;
#4832 = CARTESIAN_POINT ( 'NONE',  ( -0.3155070326520293400, -0.1306872919485614626, 0.01368055555555705224 ) ) ;
#4833 = CARTESIAN_POINT ( 'NONE',  ( -0.1116596296178200276, 0.3473214284738860846, 0.3436530038418508792 ) ) ;
#4834 = AXIS2_PLACEMENT_3D ( 'NONE', #22683, #19033, #5973 ) ;
#4835 = CARTESIAN_POINT ( 'NONE',  ( 1.679791495769851560E-14, 3.793833333485275183, 0.3119999999999999996 ) ) ;
#4836 = CARTESIAN_POINT ( 'NONE',  ( 0.1116596296178199860, 0.2223214284738861402, -0.3436530038418508792 ) ) ;
#4837 = EDGE_CURVE ( 'NONE', #13879, #17157, #9512, .T. ) ;
#4838 = EDGE_CURVE ( 'NONE', #13969, #4661, #8495, .T. ) ;
#4839 = DIRECTION ( 'NONE',  ( 1.000000000000000000, 0.000000000000000000, 0.000000000000000000 ) ) ;
#4840 = CARTESIAN_POINT ( 'NONE',  ( 0.2764156081756483641, -0.1144950937579611167, 0.06402777777777945989 ) ) ;
#4841 = CARTESIAN_POINT ( 'NONE',  ( 0.4805070082343983473, -0.2560807851245830435, 0.04413116910601658921 ) ) ;
#4842 = CARTESIAN_POINT ( 'NONE',  ( -0.1167790944451423257, 5.245222222298087544, -0.2819296736111110424 ) ) ;
#4843 = CARTESIAN_POINT ( 'NONE',  ( -0.2764156081756484196, 1.692557448933383907E-17, 0.3175000000000036682 ) ) ;
#4844 = ORIENTED_EDGE ( 'NONE', *, *, #10204, .T. ) ;
#4845 = CARTESIAN_POINT ( 'NONE',  ( -0.3125000000000000000, 1.913510623667739771E-17, 0.005000000000001014917 ) ) ;
#4846 = CARTESIAN_POINT ( 'NONE',  ( 0.06335377612981431261, 0.1303123470876126344, -0.4000000000000000777 ) ) ;
#4847 = PLANE ( 'NONE',  #20348 ) ;
#4848 = CARTESIAN_POINT ( 'NONE',  ( 1.910449006669871087E-17, 0.4208333333333330040, -0.3119999999999999996 ) ) ;
#4849 = CARTESIAN_POINT ( 'NONE',  ( -0.3119999999999999996, 4.995222222222221120, 0.000000000000000000 ) ) ;
#4850 = CARTESIAN_POINT ( 'NONE',  ( -0.2819296736111110979, 4.130638888964754507, 0.000000000000000000 ) ) ;
#4851 = CARTESIAN_POINT ( 'NONE',  ( 5.178964085587577574E-17, 3.991750000075865223, 0.2819296736111110979 ) ) ;
#4852 = EDGE_CURVE ( 'NONE', #3183, #21365, #11015, .T. ) ;
#4853 = CARTESIAN_POINT ( 'NONE',  ( 4.898587196589413075E-17, 3.700000000000000622, 0.4000000000000000222 ) ) ;
#4854 = CARTESIAN_POINT ( 'NONE',  ( 0.000000000000000000, 0.000000000000000000, 0.000000000000000000 ) ) ;
#4855 = DIRECTION ( 'NONE',  ( 0.000000000000000000, 0.000000000000000000, 1.000000000000000000 ) ) ;
#4856 = LOCAL_TIME ( 21, 9, 13.00000000000000000, #14962 ) ;
#4857 = VERTEX_POINT ( 'NONE', #15340 ) ;
#4858 = CARTESIAN_POINT ( 'NONE',  ( 0.2782497666485165277, 0.06249891821425377497, 0.1411420113220940853 ) ) ;
#4859 = CARTESIAN_POINT ( 'NONE',  ( 0.1167790944451424368, 4.425777777853643791, 0.2819296736111110424 ) ) ;
#4860 = CARTESIAN_POINT ( 'NONE',  ( -0.2923287055106771337, 0.02232142847388617762, -0.2123892367102620804 ) ) ;
#4861 = CARTESIAN_POINT ( 'NONE',  ( 0.3530939849935350594, 1.999640111863030478, -2.889019982092019045 ) ) ;
#4862 = VECTOR ( 'NONE', #6885, 39.37007874015748143 ) ;
#4863 = MECHANICAL_CONTEXT ( 'NONE', #6704, 'mechanical' ) ;
#4864 = DIRECTION ( 'NONE',  ( -0.000000000000000000, -1.000000000000000000, -0.000000000000000000 ) ) ;
#4865 = CARTESIAN_POINT ( 'NONE',  ( -0.1954553509668046918, -0.1954553509668046640, -0.01583333333333228690 ) ) ;
#4866 = CARTESIAN_POINT ( 'NONE',  ( -0.1993543840281266355, 4.095916666742533074, 0.1993543840281267465 ) ) ;
#4867 = SECURITY_CLASSIFICATION_LEVEL ( 'unclassified' ) ;
#4868 = CARTESIAN_POINT ( 'NONE',  ( -0.02489526420108369512, 4.822334970157831968, -0.3110451136060463639 ) ) ;
#4869 = CARTESIAN_POINT ( 'NONE',  ( 0.3950000000000000733, 2.978485840173427324, -0.6605837454876625214 ) ) ;
#4870 = CARTESIAN_POINT ( 'NONE',  ( -0.2764156081756484196, 0.1144950937579609918, 0.2029166666666694097 ) ) ;
#4871 = LOCAL_TIME ( 21, 9, 13.00000000000000000, #16755 ) ;
#4872 = CARTESIAN_POINT ( 'NONE',  ( 2.326421213736078119E-17, 0.02946428561674331245, -0.3799334167787516425 ) ) ;
#4873 = CARTESIAN_POINT ( 'NONE',  ( 0.2819296736111110424, -0.01666666674253329886, -0.1167790944451423119 ) ) ;
#4874 = CARTESIAN_POINT ( 'NONE',  ( -0.2973707438694075944, 0.01885122216165719539, 0.4090374105360744528 ) ) ;
#4875 = CARTESIAN_POINT ( 'NONE',  ( 0.000000000000000000, 0.4997679491924311157, 0.000000000000000000 ) ) ;
#4876 = CARTESIAN_POINT ( 'NONE',  ( -0.2723623684625769426, 0.3840173906162817064, 0.09139303015897914939 ) ) ;
#4877 = CARTESIAN_POINT ( 'NONE',  ( -3.385114897866767815E-17, -0.2764156081756484196, -0.06444444444444379083 ) ) ;
#4878 = CARTESIAN_POINT ( 'NONE',  ( 0.2230971623002953874, -0.2230971623002954429, 0.3053472222222256005 ) ) ;
#4879 = VERTEX_POINT ( 'NONE', #11806 ) ;
#4880 = EDGE_LOOP ( 'NONE', ( #17383, #1045, #8185, #8434, #11084, #11761, #6330, #10754 ) ) ;
#4881 = CYLINDRICAL_SURFACE ( 'NONE', #6766, 0.3119999999999999996 ) ;
#4882 = CARTESIAN_POINT ( 'NONE',  ( -0.1571243772177107201, 3.826150417953878780, -0.2726240822627857274 ) ) ;
#4883 = CARTESIAN_POINT ( 'NONE',  ( -0.2819296736111110424, 0.4486111110352445364, -0.1167790944451423396 ) ) ;
#4884 = CARTESIAN_POINT ( 'NONE',  ( 0.1993543840281267465, 3.998694444520310753, 0.1993543840281266633 ) ) ;
#4885 = CARTESIAN_POINT ( 'NONE',  ( 0.2472135954999579166, 0.4517857140906294533, 0.3402603233408160732 ) ) ;
#4886 = EDGE_CURVE ( 'NONE', #12390, #1032, #22529, .T. ) ;
#4887 = AXIS2_PLACEMENT_3D ( 'NONE', #10325, #12282, #12403 ) ;
#4888 = ORIENTED_EDGE ( 'NONE', *, *, #6476, .F. ) ;
#4889 = CARTESIAN_POINT ( 'NONE',  ( -0.1993543840281266910, 4.637583333409199149, -0.1993543840281266910 ) ) ;
#4890 = ADVANCED_FACE ( 'NONE', ( #20944 ), #17287, .T. ) ;
#4891 = CARTESIAN_POINT ( 'NONE',  ( 0.3041335845296361806, 5.131942972423729543, -0.03838084752963767665 ) ) ;
#4892 = CARTESIAN_POINT ( 'NONE',  ( 0.1120921421618772951, 5.088976381486351563, -0.2921505626564902536 ) ) ;
#4893 = VERTEX_POINT ( 'NONE', #22886 ) ;
#4894 = CARTESIAN_POINT ( 'NONE',  ( -0.2819296736111110424, 5.078555555631420582, 0.1167790944451424923 ) ) ;
#4895 = SECURITY_CLASSIFICATION ( '', '', #14789 ) ;
#4896 = CARTESIAN_POINT ( 'NONE',  ( 0.2769513040667488379, 4.192351017494014620, 0.1439006775907332447 ) ) ;
#4897 = ORIENTED_EDGE ( 'NONE', *, *, #5712, .F. ) ;
#4898 = CONICAL_SURFACE ( 'NONE', #8014, 0.4625000000000000777, 0.7853981633974498333 ) ;
#4899 = CARTESIAN_POINT ( 'NONE',  ( 0.2819296736111111534, 4.932722222298088433, 0.1167790944451422563 ) ) ;
#4900 = DATE_AND_TIME ( #8562, #9586 ) ;
#4901 = ORIENTED_EDGE ( 'NONE', *, *, #9910, .F. ) ;
#4902 = CIRCLE ( 'NONE', #8798, 0.3125000000000001665 ) ;
#4903 = CARTESIAN_POINT ( 'NONE',  ( -0.04028049885296762500, 5.101242447252128720, -0.3082635314558828665 ) ) ;
#4904 = CARTESIAN_POINT ( 'NONE',  ( -0.1019862276394089551, 4.568705723659588713, 0.2955327530433858318 ) ) ;
#4905 = EDGE_LOOP ( 'NONE', ( #17407, #17243, #6803, #7105, #20292 ) ) ;
#4906 = CARTESIAN_POINT ( 'NONE',  ( -0.1993543840281266633, 0.4034722221463555858, -0.1993543840281266910 ) ) ;
#4907 = EDGE_LOOP ( 'NONE', ( #11581, #4951, #10524, #2307 ) ) ;
#4908 = CARTESIAN_POINT ( 'NONE',  ( 0.1993543840281266355, 0.04236111103524448085, 0.1993543840281267465 ) ) ;
#4909 = CARTESIAN_POINT ( 'NONE',  ( 2.325416254512337577, 2.978485840173427324, -2.591000000000000636 ) ) ;
#4910 = CARTESIAN_POINT ( 'NONE',  ( -0.5116234456863466562, 0.9548081934128056503, 2.635972749958888528 ) ) ;
#4911 = CARTESIAN_POINT ( 'NONE',  ( -0.2923287055106771337, 0.1651785713310290060, -0.2123892367102620804 ) ) ;
#4912 = CARTESIAN_POINT ( 'NONE',  ( -0.2294867466249408405, 5.064319674093950674, 0.2113761149445206045 ) ) ;
#4913 = LINE ( 'NONE', #20275, #7553 ) ;
#4914 = LOCAL_TIME ( 21, 9, 13.00000000000000000, #11852 ) ;
#4915 = CARTESIAN_POINT ( 'NONE',  ( 0.2730879860166738338, 4.111524471938507119, -3.027594437230249902 ) ) ;
#4916 = CARTESIAN_POINT ( 'NONE',  ( -0.1993543840281266910, 4.693138888964754507, -0.1993543840281266910 ) ) ;
#4917 = CYLINDRICAL_SURFACE ( 'NONE', #11719, 0.3119999999999999996 ) ;
#4918 = CARTESIAN_POINT ( 'NONE',  ( 0.2819296736111110979, 3.880638888964754063, -3.452642723725051716E-17 ) ) ;
#4919 = CARTESIAN_POINT ( 'NONE',  ( 0.4687500000000003886, -0.04388698013647539253, 0.09139229829490853885 ) ) ;
#4920 = CARTESIAN_POINT ( 'NONE',  ( 0.1902774475453257452, 5.021827821991241336, 0.2506361051183713107 ) ) ;
#4921 = CARTESIAN_POINT ( 'NONE',  ( -0.4788479876972301374, -0.2689986204937560021, 0.04193567535760926723 ) ) ;
#4922 = DIRECTION ( 'NONE',  ( -0.4999999999999918954, -0.000000000000000000, -0.8660254037844432595 ) ) ;
#4923 = CARTESIAN_POINT ( 'NONE',  ( 0.3119999999999999996, 4.196611111262843252, -3.820898013339742174E-17 ) ) ;
#4924 = CARTESIAN_POINT ( 'NONE',  ( 0.1167790944451422702, 4.738277777853642903, -0.2819296736111110979 ) ) ;
#4925 =( BOUNDED_CURVE ( )  B_SPLINE_CURVE ( 2, ( #1841, #24029, #14543, #21965, #12969, #14903, #22088, #20146, #7339 ),
 .UNSPECIFIED., .F., .F. ) 
 B_SPLINE_CURVE_WITH_KNOTS ( ( 3, 2, 2, 2, 3 ),
 ( 0.6041666666666666297, 0.6145833333333333703, 0.6250000000000000000, 0.6354166666666666297, 0.6458333333333333703 ),
 .UNSPECIFIED. ) 
 CURVE ( )  GEOMETRIC_REPRESENTATION_ITEM ( )  RATIONAL_B_SPLINE_CURVE ( ( 1.000000000000000000, 0.9238795325112867385, 1.000000000000000000, 0.9238795325112867385, 1.000000000000000000, 0.9238795325112867385, 1.000000000000000000, 0.9238795325112867385, 1.000000000000000000 ) ) 
 REPRESENTATION_ITEM ( '' )  );
#4926 = CARTESIAN_POINT ( 'NONE',  ( 0.1167790944451422702, 4.168833333409199149, -0.2819296736111110424 ) ) ;
#4927 = ADVANCED_FACE ( 'NONE', ( #19112 ), #5821, .T. ) ;
#4928 = PERSON_AND_ORGANIZATION_ROLE ( 'design_supplier' ) ;
#4929 = CARTESIAN_POINT ( 'NONE',  ( -0.4209440094115188824, -0.2863418823927886270, 0.4064695056028755915 ) ) ;
#4930 = CARTESIAN_POINT ( 'NONE',  ( -0.02441201398332129568, 4.111524471938507119, -3.542879552481994043 ) ) ;
#4931 = ORIENTED_EDGE ( 'NONE', *, *, #2306, .T. ) ;
#4932 = CARTESIAN_POINT ( 'NONE',  ( -0.2206173157302027954, 0.3652777776260448528, -0.2206173157302028232 ) ) ;
#4933 = LINE ( 'NONE', #8711, #16363 ) ;
#4934 = CC_DESIGN_PERSON_AND_ORGANIZATION_ASSIGNMENT ( #18669, #9407, ( #6483 ) ) ;
#4935 = CARTESIAN_POINT ( 'NONE',  ( -0.4687500000000003886, -0.04441404256795419142, 0.4171848040509457123 ) ) ;
#4937 = EDGE_CURVE ( 'NONE', #12807, #7226, #10378, .T. ) ;
#4936 = CARTESIAN_POINT ( 'NONE',  ( 0.1704550048180128174, 0.2392892945790311421, -0.7304142363202623667 ) ) ;
#4938 = VERTEX_POINT ( 'NONE', #6181 ) ;
#4939 = FACE_OUTER_BOUND ( 'NONE', #908, .T. ) ;
#4940 = DIRECTION ( 'NONE',  ( 0.000000000000000000, 0.000000000000000000, 1.000000000000000000 ) ) ;
#4941 = CARTESIAN_POINT ( 'NONE',  ( -0.2764156081756484196, 1.692557448933383907E-17, 0.08833333333333522053 ) ) ;
#4942 = CARTESIAN_POINT ( 'NONE',  ( 0.1993543840281266633, 4.387583333409199149, -0.1993543840281266910 ) ) ;
#4943 = CARTESIAN_POINT ( 'NONE',  ( -0.2209708691207961373, -0.2209708691207961095, 0.4008333333333374826 ) ) ;
#4944 = CARTESIAN_POINT ( 'NONE',  ( -0.1015928384594063510, 0.7712678869592031194, -1.079846914997397489 ) ) ;
#4945 = CARTESIAN_POINT ( 'NONE',  ( -0.09435543239135868454, -0.003009961218012348859, 2.763260016782451700 ) ) ;
#4946 = CARTESIAN_POINT ( 'NONE',  ( 0.3003475124358450099, 4.111524471938507119, -3.730379552481990491 ) ) ;
#4947 = CARTESIAN_POINT ( 'NONE',  ( 0.2206173157302028787, 4.071611111111110404, 0.2206173157302027954 ) ) ;
#4948 = CARTESIAN_POINT ( 'NONE',  ( 0.2206173157302028787, 4.911888889040620931, 0.2206173157302027954 ) ) ;
#4949 = AXIS2_PLACEMENT_3D ( 'NONE', #10537, #23554, #21498 ) ;
#4950 = CARTESIAN_POINT ( 'NONE',  ( -1.062695237341364068E-12, 5.118312382271687611, 0.3086920601714014945 ) ) ;
#4951 = ORIENTED_EDGE ( 'NONE', *, *, #20650, .F. ) ;
#4952 = CARTESIAN_POINT ( 'NONE',  ( -0.3119535588213346866, 4.892301757544008645, 0.04116472303791206266 ) ) ;
#4953 = B_SPLINE_CURVE_WITH_KNOTS ( 'NONE', 3,
 ( #13841, #13726, #15783, #663, #15427, #11773, #7977, #4202, #12021, #782, #15308, #22737, #19435, #8212, #22855, #21148, #4436, #6144, #15661, #6025, #11655, #21026, #23080, #4318, #11903, #23201, #6512, #4679, #13493, #20908, #10063, #6389, #19193, #19321, #2503, #19079, #2620, #8090, #2386, #13611, #6268, #17257, #15544, #17610, #2735, #541 ),
 .UNSPECIFIED., .F., .F.,
 ( 4, 2, 2, 2, 2, 2, 2, 2, 2, 2, 2, 2, 2, 2, 2, 2, 2, 2, 2, 2, 2, 2, 4 ),
 ( 0.005337107837582267221, 0.006801130698153545241, 0.008265153558724824129, 0.008997164989010464006, 0.009729176419296105618, 0.01119319927986738884, 0.01192521071015302872, 0.01265722214043866686, 0.01412124500100994315, 0.01558526786158121596, 0.01631727929186685411, 0.01704929072215248878, 0.01851331358272376854, 0.01997733644329504829, 0.02144135930386632805, 0.02217337073415196619, 0.02290538216443760780, 0.02363739359472324594, 0.02436940502500888409, 0.02583342788558016037, 0.02656543931586579851, 0.02729745074615143666, 0.02876147360672271294 ),
 .UNSPECIFIED. ) ;
#4954 = CARTESIAN_POINT ( 'NONE',  ( 0.3155070326520292290, 0.1306872919485615736, -0.06965277777777696688 ) ) ;
#4955 = DIRECTION ( 'NONE',  ( -0.4999999999999995559, 0.8660254037844389297, 0.000000000000000000 ) ) ;
#4956 = DIRECTION ( 'NONE',  ( 0.000000000000000000, -0.000000000000000000, 1.000000000000000000 ) ) ;
#4957 = ADVANCED_FACE ( 'NONE', ( #13400 ), #19407, .T. ) ;
#4958 = CARTESIAN_POINT ( 'NONE',  ( -0.1116596296178199582, 0.1580357141881718608, -0.3436530038418508792 ) ) ;
#4959 = CARTESIAN_POINT ( 'NONE',  ( -0.2819296736111110979, 0.1326388888130222710, -3.452642723725051716E-17 ) ) ;
#4960 = CARTESIAN_POINT ( 'NONE',  ( 0.1144950937579611444, 0.2764156081756483641, -0.03319444444444354797 ) ) ;
#4961 = CARTESIAN_POINT ( 'NONE',  ( 0.3613381517857143232, 0.2223214284738861402, 0.1174058825155741975 ) ) ;
#4962 = CARTESIAN_POINT ( 'NONE',  ( 0.1993543840281267465, 5.220916666742532186, 0.1993543840281266633 ) ) ;
#4963 = CARTESIAN_POINT ( 'NONE',  ( -3.385114897866767815E-17, -0.2764156081756484196, 0.3313888888888926743 ) ) ;
#4964 = DIRECTION ( 'NONE',  ( -0.000000000000000000, -1.000000000000000000, -0.000000000000000000 ) ) ;
#4965 = CARTESIAN_POINT ( 'NONE',  ( -0.1593056001970055702, 4.270767213191519751, -0.2687184019925401568 ) ) ;
#4966 = LINE ( 'NONE', #21914, #13748 ) ;
#4967 = CARTESIAN_POINT ( 'NONE',  ( -0.1292346314604056190, 0.5354166666666662078, -0.3119999999999999996 ) ) ;
#4968 = CARTESIAN_POINT ( 'NONE',  ( -1.910449006669871087E-17, 4.814666666666665762, -0.3119999999999999996 ) ) ;
#4969 = CARTESIAN_POINT ( 'NONE',  ( -0.1993543840281266910, 4.290361111186976828, -0.1993543840281266910 ) ) ;
#4970 = CARTESIAN_POINT ( 'NONE',  ( 0.000000000000000000, 2.740000000000000213, 0.000000000000000000 ) ) ;
#4971 = CARTESIAN_POINT ( 'NONE',  ( 0.000000000000000000, 3.738758431839877614E-19, -0.1145082521472477743 ) ) ;
#4972 = CARTESIAN_POINT ( 'NONE',  ( 0.1292346314604082835, 4.401472222222221120, 0.3119999999999974460 ) ) ;
#4973 = FACE_OUTER_BOUND ( 'NONE', #1688, .T. ) ;
#4974 = CARTESIAN_POINT ( 'NONE',  ( -0.1993543840281266355, 4.526472222298087544, 0.1993543840281267465 ) ) ;
#4975 = EDGE_CURVE ( 'NONE', #5171, #9466, #15602, .T. ) ;
#4976 = EDGE_CURVE ( 'NONE', #1526, #848, #8904, .T. ) ;
#4977 = CARTESIAN_POINT ( 'NONE',  ( 0.4593750000000003664, -0.2760455974562899817, 0.06112444011295372487 ) ) ;
#4978 = EDGE_CURVE ( 'NONE', #3235, #20999, #11620, .T. ) ;
#4979 = EDGE_CURVE ( 'NONE', #6926, #5016, #13521, .T. ) ;
#4980 = VECTOR ( 'NONE', #21329, 39.37007874015748143 ) ;
#4981 = APPROVAL_STATUS ( 'not_yet_approved' ) ;
#4982 = DIRECTION ( 'NONE',  ( 0.000000000000000000, 0.000000000000000000, -1.000000000000000000 ) ) ;
#4983 = CARTESIAN_POINT ( 'NONE',  ( 0.1144950937579609085, -0.2764156081756484751, 0.1056944444444464504 ) ) ;
#4984 = CARTESIAN_POINT ( 'NONE',  ( 0.1993543840281266633, 4.179250000075865223, -0.1993543840281266910 ) ) ;
#4985 = CARTESIAN_POINT ( 'NONE',  ( 1.312321497832610059E-07, 4.821611112096344520, -0.3119999999999724105 ) ) ;
#4986 = ADVANCED_FACE ( 'NONE', ( #11892 ), #9438, .T. ) ;
#4987 = DIRECTION ( 'NONE',  ( -0.5000000000000012212, 0.8660254037844380415, 0.000000000000000000 ) ) ;
#4988 = CARTESIAN_POINT ( 'NONE',  ( 0.1954553509668046640, -0.1954553509668047195, 0.2272222222222252119 ) ) ;
#4989 = CARTESIAN_POINT ( 'NONE',  ( 0.2233192592356399997, -0.04910714295468525392, -0.3073725909049500049 ) ) ;
#4990 = CARTESIAN_POINT ( 'NONE',  ( 0.1993543840281266355, 0.5979166665908000056, 0.1993543840281267465 ) ) ;
#4991 = CARTESIAN_POINT ( 'NONE',  ( -0.09987075367823573802, 0.2738295200956166187, 0.4025228681615854454 ) ) ;
#4992 = CARTESIAN_POINT ( 'NONE',  ( -0.4796770409652741929, 0.08628438008767304324, 0.07157438297392351712 ) ) ;
#4993 = CARTESIAN_POINT ( 'NONE',  ( 0.000000000000000000, 3.738758431839877614E-19, 0.000000000000000000 ) ) ;
#4994 = CARTESIAN_POINT ( 'NONE',  ( -0.2764156081756484196, 0.1144950937579609918, 0.08486111111111295513 ) ) ;
#4995 = CARTESIAN_POINT ( 'NONE',  ( -0.2230971623002953874, 0.2230971623002954152, 0.3331250000000036127 ) ) ;
#4996 = ORIENTED_EDGE ( 'NONE', *, *, #6639, .T. ) ;
#4997 = ORIENTED_EDGE ( 'NONE', *, *, #8124, .F. ) ;
#4998 = CARTESIAN_POINT ( 'NONE',  ( 3.857637417314162073E-17, 0.1199999999999999956, 0.3150000000000000022 ) ) ;
#4999 = CARTESIAN_POINT ( 'NONE',  ( -0.3119999807755027277, 3.834402680349659143, -0.04084143460943073095 ) ) ;
#5000 = CARTESIAN_POINT ( 'NONE',  ( -0.2819296736111110979, 0.4520833332574666907, -3.452642723725051716E-17 ) ) ;
#5001 = CARTESIAN_POINT ( 'NONE',  ( 0.2819296736111110424, 3.898000000075866112, -0.1167790944451423396 ) ) ;
#5002 = VECTOR ( 'NONE', #5783, 39.37007874015748143 ) ;
#5003 = CARTESIAN_POINT ( 'NONE',  ( -0.3613381517857143232, 0.04732142847388616513, -4.425116109941954795E-17 ) ) ;
#5004 = ORIENTED_EDGE ( 'NONE', *, *, #15741, .F. ) ;
#5005 = CARTESIAN_POINT ( 'NONE',  ( -0.1993543840281266910, 4.748694444520309865, -0.1993543840281266910 ) ) ;
#5006 = FACE_OUTER_BOUND ( 'NONE', #16300, .T. ) ;
#5007 = CARTESIAN_POINT ( 'NONE',  ( 5.731347020009612645E-17, 3.897999999999999243, 0.3119999999999999996 ) ) ;
#5008 = EDGE_LOOP ( 'NONE', ( #22575, #4516, #9952, #13940 ) ) ;
#5009 = B_SPLINE_CURVE_WITH_KNOTS ( 'NONE', 3,
 ( #23957, #23588, #19951, #10814, #8972, #21895, #5184, #16295, #5062, #12532, #16538, #3241, #12655, #5312, #8849, #10933, #9089, #3362, #18361, #1654, #14719, #11051, #7271, #9218, #16420, #23829, #22133, #7387, #10575, #5434, #18480, #14839, #3599, #5552, #12899, #20315, #19829, #18005, #3124, #8722 ),
 .UNSPECIFIED., .F., .F.,
 ( 4, 2, 1, 2, 2, 1, 2, 2, 2, 2, 2, 2, 1, 1, 2, 2, 2, 2, 2, 2, 2, 4 ),
 ( 0.6487731362554981507, 0.6493439294636441650, 0.6494866277656805575, 0.6495579769166988093, 0.6495936514922079352, 0.6496293260677170611, 0.6499147226717900683, 0.6510563090880819859, 0.6521978955043739035, 0.6533394819206658211, 0.6556226547532496562, 0.6567642411695416849, 0.6569069394715780774, 0.6569782886225963292, 0.6570139631981054551, 0.6570496377736145810, 0.6573350343776875881, 0.6579058275858336025, 0.6601890004184174376, 0.6624721732510013839, 0.6647553460835852190, 0.6670385189161691653 ),
 .UNSPECIFIED. ) ;
#5010 = LINE ( 'NONE', #8428, #5037 ) ;
#5011 = CARTESIAN_POINT ( 'NONE',  ( 0.2819296736111110979, 5.210500000075865223, 0.1167790944451422425 ) ) ;
#5012 = CARTESIAN_POINT ( 'NONE',  ( 2.583392422801339445E-17, 0.8699999999999998845, 0.2109499999999998043 ) ) ;
#5013 = CARTESIAN_POINT ( 'NONE',  ( 0.1236067977499789861, 0.2624999998049151739, -0.3804226065180614236 ) ) ;
#5014 = CARTESIAN_POINT ( 'NONE',  ( -0.1167790944451423535, 4.974388888964754507, 0.2819296736111110979 ) ) ;
#5015 = APPROVAL_DATE_TIME ( #14297, #3454 ) ;
#5016 = VERTEX_POINT ( 'NONE', #9932 ) ;
#5017 = ADVANCED_FACE ( 'NONE', ( #11643 ), #11521, .T. ) ;
#5018 = CARTESIAN_POINT ( 'NONE',  ( -0.3051426028078303987, 5.113331766849443127, -0.05202755180939230145 ) ) ;
#5019 = CARTESIAN_POINT ( 'NONE',  ( -0.2802025597200765161, 4.561924260886437210, 0.1428905893484782030 ) ) ;
#5020 = ORIENTED_EDGE ( 'NONE', *, *, #17624, .T. ) ;
#5021 = CARTESIAN_POINT ( 'NONE',  ( -0.1993543840281267465, 0.1951388888130222710, 0.1993543840281266633 ) ) ;
#5022 = ORIENTED_EDGE ( 'NONE', *, *, #7369, .T. ) ;
#5023 = DIRECTION ( 'NONE',  ( -0.000000000000000000, 1.000000000000000000, -0.000000000000000000 ) ) ;
#5024 = CARTESIAN_POINT ( 'NONE',  ( -0.2499688240500823333, 4.730080733492335376, 0.1894356414185249249 ) ) ;
#5025 = CARTESIAN_POINT ( 'NONE',  ( -0.2748157666139303124, 5.203214401271618605, 0.07108222885202038210 ) ) ;
#5026 = CARTESIAN_POINT ( 'NONE',  ( -0.3236067977499790249, 0.01428571428571426098, 0.2351141009169892271 ) ) ;
#5027 = CARTESIAN_POINT ( 'NONE',  ( -0.3009011790701222600, 5.060279419410155022, 0.08637144214764777561 ) ) ;
#5028 = DIRECTION ( 'NONE',  ( 0.000000000000000000, 0.000000000000000000, 1.000000000000000000 ) ) ;
#5029 = CARTESIAN_POINT ( 'NONE',  ( -0.2564683202935754691, 3.885663880049097241, -0.1776738855868679468 ) ) ;
#5030 = DIRECTION ( 'NONE',  ( -0.8660254037844501429, -0.000000000000000000, 0.4999999999999801270 ) ) ;
#5031 = CARTESIAN_POINT ( 'NONE',  ( -0.1993543840281266910, 4.748694444520309865, -0.1993543840281266910 ) ) ;
#5032 = CARTESIAN_POINT ( 'NONE',  ( 0.07186756554182434364, 4.518106518300164964, 0.3043097197694309974 ) ) ;
#5033 = CARTESIAN_POINT ( 'NONE',  ( -0.2819296736111110424, 3.738277777853643347, -0.1167790944451423119 ) ) ;
#5034 = CARTESIAN_POINT ( 'NONE',  ( -0.2274437723577396042, 0.04798558205255324532, -0.1920016971050759469 ) ) ;
#5035 = CARTESIAN_POINT ( 'NONE',  ( 0.2859772800003606563, 5.033587069339882092, -0.1247896800457511945 ) ) ;
#5036 = CARTESIAN_POINT ( 'NONE',  ( 0.2782497666485165277, 0.06249891821425377497, 0.1411420113220940853 ) ) ;
#5037 = VECTOR ( 'NONE', #10633, 39.37007874015748143 ) ;
#5038 = DIRECTION ( 'NONE',  ( -1.224646799147353207E-16, 1.000000000000000000, 0.000000000000000000 ) ) ;
#5039 = CARTESIAN_POINT ( 'NONE',  ( -0.2206173157302027676, 4.342444444596176290, 0.2206173157302028787 ) ) ;
#5040 = CARTESIAN_POINT ( 'NONE',  ( -0.2819296736111110424, 4.703555555631421470, 0.1167790944451424923 ) ) ;
#5041 = CARTESIAN_POINT ( 'NONE',  ( 0.1993543840281267465, 3.818138888964754507, 0.1993543840281266633 ) ) ;
#5042 = ORIENTED_EDGE ( 'NONE', *, *, #23927, .T. ) ;
#5043 = EDGE_LOOP ( 'NONE', ( #15172, #22124, #192, #21212 ) ) ;
#5044 = APPLICATION_PROTOCOL_DEFINITION ( 'international standard', 'config_control_design', 1994, #13114 ) ;
#5045 = AXIS2_PLACEMENT_3D ( 'NONE', #18283, #1696, #16458 ) ;
#5046 = CARTESIAN_POINT ( 'NONE',  ( -0.3120659000946393036, 4.945554085942006850, -0.04037676907161258377 ) ) ;
#5047 = DIRECTION ( 'NONE',  ( 0.4999999999999913403, 0.000000000000000000, -0.8660254037844437036 ) ) ;
#5048 = ORIENTED_EDGE ( 'NONE', *, *, #8124, .T. ) ;
#5049 = CARTESIAN_POINT ( 'NONE',  ( 0.3119999999999998885, 0.1743055554038226151, 0.1292346314604058410 ) ) ;
#5050 = VECTOR ( 'NONE', #9661, 39.37007874015748143 ) ;
#5051 = CARTESIAN_POINT ( 'NONE',  ( -0.2267756154094652810, 4.384351444865524527, -0.2142830584042328124 ) ) ;
#5052 = CARTESIAN_POINT ( 'NONE',  ( -0.4593750000000004219, -0.2760455974562901482, 0.4425000000000000044 ) ) ;
#5053 = CARTESIAN_POINT ( 'NONE',  ( 0.000000000000000000, 5.384999999999999787, 0.000000000000000000 ) ) ;
#5054 = CARTESIAN_POINT ( 'NONE',  ( 0.05567750539902905499, 0.5846369443820266243, -0.7480565307454484225 ) ) ;
#5055 = ORIENTED_EDGE ( 'NONE', *, *, #6477, .F. ) ;
#5056 = CARTESIAN_POINT ( 'NONE',  ( 0.05000000000000028727, 0.000000000000000000, -2.107450815951460221 ) ) ;
#5057 = CARTESIAN_POINT ( 'NONE',  ( 0.2819296736111110979, 0.3687499999241333759, 0.000000000000000000 ) ) ;
#5058 = CARTESIAN_POINT ( 'NONE',  ( -3.385114897866767815E-17, -0.2764156081756484196, 0.1022222222222241989 ) ) ;
#5059 = VERTEX_POINT ( 'NONE', #2123 ) ;
#5060 = CARTESIAN_POINT ( 'NONE',  ( -0.1993543840281266355, 4.359805555631421470, 0.1993543840281267465 ) ) ;
#5061 = LINE ( 'NONE', #12531, #4401 ) ;
#5062 = CARTESIAN_POINT ( 'NONE',  ( -0.04459125003299137247, 4.237043471246520809, 0.3087979979381368922 ) ) ;
#5063 = CARTESIAN_POINT ( 'NONE',  ( 0.2206173157302028787, 4.127166666666665762, 0.2206173157302027954 ) ) ;
#5064 = CARTESIAN_POINT ( 'NONE',  ( 0.1292346314604056190, 5.040361111262842364, -0.3119999999999999996 ) ) ;
#5065 = AXIS2_PLACEMENT_3D ( 'NONE', #19638, #2938, #17938 ) ;
#5066 = CONICAL_SURFACE ( 'NONE', #10161, 0.6391249999999999432, 1.134464013796309345 ) ;
#5067 = VERTEX_POINT ( 'NONE', #9812 ) ;
#5068 = CARTESIAN_POINT ( 'NONE',  ( -0.4749999999999999778, 3.575000000000000622, 2.908536147974962357E-17 ) ) ;
#5069 = ORIENTED_EDGE ( 'NONE', *, *, #8493, .F. ) ;
#5070 = CARTESIAN_POINT ( 'NONE',  ( -0.1913865654062817945, 4.883039109442649739, -0.2464053351942348535 ) ) ;
#5071 = CARTESIAN_POINT ( 'NONE',  ( 0.1306872919485616846, 0.3155070326520292290, 0.3261805555555595260 ) ) ;
#5072 = DIRECTION ( 'NONE',  ( 0.8320502943378442762, 0.4803844614152616432, -0.2773500981126125198 ) ) ;
#5073 = CARTESIAN_POINT ( 'NONE',  ( -0.4223136544080929311, -0.2974429753103077223, 0.07050986311825914454 ) ) ;
#5074 =( BOUNDED_CURVE ( )  B_SPLINE_CURVE ( 2, ( #15746, #23399, #14151, #21708, #11984, #21580, #19397, #10147, #23157 ),
 .UNSPECIFIED., .F., .T. ) 
 B_SPLINE_CURVE_WITH_KNOTS ( ( 3, 2, 2, 2, 3 ),
 ( 0.1875000000000000000, 0.1979166666666666574, 0.2083333333333333426, 0.2187500000000000000, 0.2291666666666666574 ),
 .UNSPECIFIED. ) 
 CURVE ( )  GEOMETRIC_REPRESENTATION_ITEM ( )  RATIONAL_B_SPLINE_CURVE ( ( 1.000000000000000000, 0.9238795325112867385, 1.000000000000000000, 0.9238795325112867385, 1.000000000000000000, 0.9238795325112867385, 1.000000000000000000, 0.9238795325112867385, 1.000000000000000000 ) ) 
 REPRESENTATION_ITEM ( '' )  );
#5075 = CIRCLE ( 'NONE', #8197, 0.01874999999999997502 ) ;
#5076 = CARTESIAN_POINT ( 'NONE',  ( 0.3613381517857143232, 0.2044642856167432632, 0.1174058825155742114 ) ) ;
#5077 = CIRCLE ( 'NONE', #1214, 0.4453125000000000000 ) ;
#5078 = CARTESIAN_POINT ( 'NONE',  ( -0.2819296736111110979, 0.2958333332574666907, -0.1167790944451423396 ) ) ;
#5079 = CARTESIAN_POINT ( 'NONE',  ( -0.1144950937579609918, -0.2764156081756484196, 0.1056944444444464504 ) ) ;
#5080 = CARTESIAN_POINT ( 'NONE',  ( -0.2819296736111110424, 5.141055555631421470, -0.1167790944451423119 ) ) ;
#5081 = CARTESIAN_POINT ( 'NONE',  ( 0.2135326563692477309, 4.481723286349742708, -0.2284020054868782235 ) ) ;
#5082 = EDGE_LOOP ( 'NONE', ( #14987, #4449, #1532 ) ) ;
#5083 = CARTESIAN_POINT ( 'NONE',  ( -0.008779695402981809935, 4.599642847705920801, -0.3118941039586931585 ) ) ;
#5084 = CARTESIAN_POINT ( 'NONE',  ( -4.638126268221291196E-16, 0.1321428571428571175, -0.4000000000000000222 ) ) ;
#5085 = LINE ( 'NONE', #7054, #18783 ) ;
#5086 = CARTESIAN_POINT ( 'NONE',  ( -0.4772460259542071759, 0.2717629240624621079, 0.04193793378272828859 ) ) ;
#5087 = CARTESIAN_POINT ( 'NONE',  ( -0.1292346314604057023, 4.783416666666665762, 0.3119999999999998885 ) ) ;
#5088 = EDGE_CURVE ( 'NONE', #10393, #14932, #11234, .T. ) ;
#5089 = CARTESIAN_POINT ( 'NONE',  ( -0.2819296736111110424, 3.911888888964754507, 0.1167790944451424923 ) ) ;
#5090 = CARTESIAN_POINT ( 'NONE',  ( -0.1167790944451423257, 3.800777777853643347, -0.2819296736111110424 ) ) ;
#5091 = DIRECTION ( 'NONE',  ( 0.000000000000000000, -0.000000000000000000, 1.000000000000000000 ) ) ;
#5092 = CARTESIAN_POINT ( 'NONE',  ( 0.3119999999999999996, 0.5111111109593782231, 0.000000000000000000 ) ) ;
#5093 = ORIENTED_EDGE ( 'NONE', *, *, #11572, .F. ) ;
#5094 = CYLINDRICAL_SURFACE ( 'NONE', #8150, 0.3119999999999999996 ) ;
#5095 = CARTESIAN_POINT ( 'NONE',  ( -0.1167790944451423535, 4.585500000075865223, 0.2819296736111110424 ) ) ;
#5096 = EDGE_CURVE ( 'NONE', #12983, #1519, #17361, .T. ) ;
#5097 = CARTESIAN_POINT ( 'NONE',  ( -0.3034432599227261940, 4.504371932559179115, 0.07687943905626030972 ) ) ;
#5098 = AXIS2_PLACEMENT_3D ( 'NONE', #23429, #10419, #15888 ) ;
#5099 = B_SPLINE_CURVE_WITH_KNOTS ( 'NONE', 3,
 ( #20567, #20805, #319, #2278, #9715, #7872, #22752, #18860, #441, #2400, #15202, #4217, #9839, #7992, #555, #5806, #15322, #4093, #6043, #13510, #17271, #3865, #15445, #22870, #6160, #8105, #13270, #15560, #18737, #7759, #13626, #21043, #17388, #15089, #11785, #682, #19210, #16905, #2517, #22982, #3977, #13153, #200 ),
 .UNSPECIFIED., .F., .F.,
 ( 4, 2, 2, 2, 2, 1, 1, 2, 2, 2, 2, 2, 2, 2, 2, 2, 2, 2, 2, 2, 1, 2, 4 ),
 ( 0.5208383355989948393, 0.5219801074602197222, 0.5225509933908321081, 0.5228364363561384121, 0.5228721167268016723, 0.5229077970974649325, 0.5229791578387914530, 0.5231218793214446050, 0.5254054230438944817, 0.5276889667663443584, 0.5299725104887942351, 0.5322560542112441118, 0.5333978260724689946, 0.5345395979336938774, 0.5356813697949188713, 0.5368231416561437541, 0.5373940275867562510, 0.5376794705520624440, 0.5377508312933890755, 0.5377865116640523357, 0.5378221920347155960, 0.5379649135173687480, 0.5391066853785936308 ),
 .UNSPECIFIED. ) ;
#5100 = PERSON_AND_ORGANIZATION_ROLE ( 'creator' ) ;
#5101 = CARTESIAN_POINT ( 'NONE',  ( 0.4172595264191667486, 2.291712385858714285, -0.8269699969948853813 ) ) ;
#5102 = CARTESIAN_POINT ( 'NONE',  ( -0.1954553509668046918, -0.1954553509668046640, 0.2063888888888917028 ) ) ;
#5103 = CARTESIAN_POINT ( 'NONE',  ( 0.1993543840281267465, 4.109805555631421470, 0.1993543840281266633 ) ) ;
#5104 = CARTESIAN_POINT ( 'NONE',  ( 0.000000000000000000, 5.072999999999999510, 0.000000000000000000 ) ) ;
#5105 = CARTESIAN_POINT ( 'NONE',  ( 1.337745543335387199E-07, 4.460505239618372642, 0.3119999999999396589 ) ) ;
#5106 = DIRECTION ( 'NONE',  ( 0.000000000000000000, 0.000000000000000000, -1.000000000000000000 ) ) ;
#5107 = CARTESIAN_POINT ( 'NONE',  ( -0.2233192592356399997, -0.01339285724039954162, 0.3073725909049499494 ) ) ;
#5108 = CARTESIAN_POINT ( 'NONE',  ( 1.726321361862525858E-17, -0.006250000075866632768, -0.2819296736111110979 ) ) ;
#5109 = CARTESIAN_POINT ( 'NONE',  ( 0.4687500000000002220, 0.1725658479149915492, 0.06591615843556912491 ) ) ;
#5110 = CARTESIAN_POINT ( 'NONE',  ( 0.1292346314604057300, 0.5631944444444441089, 0.3119999999999998885 ) ) ;
#5111 = CARTESIAN_POINT ( 'NONE',  ( -0.09538643074235236829, 0.1770772191347038393, -0.7440238671003180926 ) ) ;
#5112 = CARTESIAN_POINT ( 'NONE',  ( 0.1144950937579611444, 0.2764156081756483641, 0.07097222222222394905 ) ) ;
#5113 = CARTESIAN_POINT ( 'NONE',  ( 0.2230971623002953874, -0.2230971623002954429, 0.3609027777777815693 ) ) ;
#5114 = ORIENTED_EDGE ( 'NONE', *, *, #18843, .F. ) ;
#5115 = CARTESIAN_POINT ( 'NONE',  ( -0.5116234456863466562, 3.066692553488282957, 2.910369331946250249 ) ) ;
#5116 = EDGE_CURVE ( 'NONE', #7566, #2478, #4207, .T. ) ;
#5117 = CARTESIAN_POINT ( 'NONE',  ( -0.2726212559319319273, 3.830960530932576269, -0.1571292937601793949 ) ) ;
#5118 = CARTESIAN_POINT ( 'NONE',  ( 0.1167790944451423257, 0.3791666665908000611, -0.2819296736111110424 ) ) ;
#5119 = EDGE_CURVE ( 'NONE', #1058, #14932, #707, .T. ) ;
#5120 = CARTESIAN_POINT ( 'NONE',  ( -1.726321361862525858E-17, 3.741750000075865668, -0.2819296736111110979 ) ) ;
#5121 = CARTESIAN_POINT ( 'NONE',  ( 0.3613381517857143232, 0.08303571418817189131, 0.000000000000000000 ) ) ;
#5122 = ORIENTED_EDGE ( 'NONE', *, *, #385, .F. ) ;
#5123 = CARTESIAN_POINT ( 'NONE',  ( 5.178964085587577574E-17, 4.325083333409199149, 0.2819296736111110979 ) ) ;
#5124 = DIRECTION ( 'NONE',  ( -3.327464060492345934E-16, 1.000000000000000000, -5.763336813132313106E-16 ) ) ;
#5125 = LINE ( 'NONE', #5493, #23841 ) ;
#5126 = ORIENTED_EDGE ( 'NONE', *, *, #1557, .F. ) ;
#5127 = CARTESIAN_POINT ( 'NONE',  ( 0.8119709581221709049, 0.000000000000000000, -1.327785115251736814 ) ) ;
#5128 = CARTESIAN_POINT ( 'NONE',  ( 0.2819296736111110979, 5.158416666742532186, -3.452642723725051716E-17 ) ) ;
#5129 = EDGE_CURVE ( 'NONE', #9589, #23206, #22612, .T. ) ;
#5130 =( BOUNDED_CURVE ( )  B_SPLINE_CURVE ( 2, ( #16605, #16367, #9405, #5621, #12843, #11118, #12724, #13085, #9281 ),
 .UNSPECIFIED., .F., .F. ) 
 B_SPLINE_CURVE_WITH_KNOTS ( ( 3, 2, 2, 2, 3 ),
 ( 0.1696428571428572063, 0.1741071428571428215, 0.1785714285714284644, 0.1830357142857140795, 0.1874999999999997224 ),
 .UNSPECIFIED. ) 
 CURVE ( )  GEOMETRIC_REPRESENTATION_ITEM ( )  RATIONAL_B_SPLINE_CURVE ( ( 0.9999999999999990008, 0.9238795325112877377, 1.000000000000000000, 0.9238795325112867385, 1.000000000000000000, 0.9238795325112867385, 1.000000000000000000, 0.9238795325112915124, 0.9999999999999952260 ) ) 
 REPRESENTATION_ITEM ( '' )  );
#5131 = CARTESIAN_POINT ( 'NONE',  ( -1.960390272410463459E-06, 4.210500054279665783, -0.3119999999938410928 ) ) ;
#5132 =( NAMED_UNIT ( * ) SI_UNIT ( $, .STERADIAN. ) SOLID_ANGLE_UNIT ( ) );
#5133 = LINE ( 'NONE', #23897, #18923 ) ;
#5134 = CARTESIAN_POINT ( 'NONE',  ( 0.1167790944451422702, 4.946611111186975940, -0.2819296736111110979 ) ) ;
#5135 = SECURITY_CLASSIFICATION_LEVEL ( 'unclassified' ) ;
#5136 = VERTEX_POINT ( 'NONE', #7847 ) ;
#5137 = CARTESIAN_POINT ( 'NONE',  ( 1.573500000000000343, 0.05625000000000004996, -1.006250000000000311 ) ) ;
#5138 = CARTESIAN_POINT ( 'NONE',  ( -0.06344784419188649605, 4.569835828710965941, 0.3056428810798353934 ) ) ;
#5139 = ORIENTED_EDGE ( 'NONE', *, *, #23240, .T. ) ;
#5140 = CARTESIAN_POINT ( 'NONE',  ( -0.2819296736111110979, 0.2472222221463555580, 0.1167790944451422425 ) ) ;
#5141 = ORIENTED_EDGE ( 'NONE', *, *, #6540, .F. ) ;
#5142 = CARTESIAN_POINT ( 'NONE',  ( 0.1993543840281266355, 0.09791666659080004720, 0.1993543840281267465 ) ) ;
#5143 = CYLINDRICAL_SURFACE ( 'NONE', #10018, 0.3125000000000000000 ) ;
#5144 = CARTESIAN_POINT ( 'NONE',  ( -0.4466234456863466540, 0.6134519301839026495, 2.586897977077770250 ) ) ;
#5145 = CARTESIAN_POINT ( 'NONE',  ( -6.979263641208234666E-17, 0.4044642856167431355, 0.3799334167787516425 ) ) ;
#5146 = CARTESIAN_POINT ( 'NONE',  ( -0.3125000000000000000, 0.000000000000000000, 1.326383476483184332 ) ) ;
#5147 = CIRCLE ( 'NONE', #9849, 0.3149999999999999467 ) ;
#5148 = CARTESIAN_POINT ( 'NONE',  ( 0.3124999999999996669, 0.04488961648801697429, 0.4228708124548387071 ) ) ;
#5149 = CARTESIAN_POINT ( 'NONE',  ( 0.000000000000000000, 0.4199999999999998734, 0.000000000000000000 ) ) ;
#5150 = CARTESIAN_POINT ( 'NONE',  ( -0.3125000000000000000, 0.000000000000000000, 1.326383476483184332 ) ) ;
#5151 = EDGE_CURVE ( 'NONE', #14891, #14020, #11948, .T. ) ;
#5152 = CARTESIAN_POINT ( 'NONE',  ( -0.1993543840281266910, 4.415361111186976828, -0.1993543840281266910 ) ) ;
#5153 = FACE_OUTER_BOUND ( 'NONE', #10, .T. ) ;
#5154 = CARTESIAN_POINT ( 'NONE',  ( -0.2206173157302028787, 0.2680555554038226429, 0.2206173157302027954 ) ) ;
#5155 = CARTESIAN_POINT ( 'NONE',  ( 0.2819296736111110979, 5.116750000075866112, -3.452642723725051716E-17 ) ) ;
#5156 = CARTESIAN_POINT ( 'NONE',  ( 0.4687500000000003886, -0.1740109699597048587, 0.07813294176666470137 ) ) ;
#5157 = CARTESIAN_POINT ( 'NONE',  ( 0.2727877922144690270, 4.923470271033195012, -0.1568345301858280472 ) ) ;
#5158 = CARTESIAN_POINT ( 'NONE',  ( 0.2530624153226711526, 5.072996518863750026, 0.1824922298374807572 ) ) ;
#5159 = ORIENTED_EDGE ( 'NONE', *, *, #13931, .F. ) ;
#5160 = CARTESIAN_POINT ( 'NONE',  ( -0.1206821249410769403, 4.790362928687555311, 0.2884035782607159981 ) ) ;
#5161 = CARTESIAN_POINT ( 'NONE',  ( 5.731347020009612645E-17, 4.293833333485065573, 0.3119999999999999996 ) ) ;
#5162 = ADVANCED_FACE ( 'NONE', ( #11667 ), #18243, .T. ) ;
#5163 = CARTESIAN_POINT ( 'NONE',  ( -1.726321361862525858E-17, 4.463972222298087544, -0.2819296736111110979 ) ) ;
#5164 = CARTESIAN_POINT ( 'NONE',  ( 0.2819296736111110979, 3.825083333409198705, -3.452642723725051716E-17 ) ) ;
#5165 = VERTEX_POINT ( 'NONE', #17385 ) ;
#5166 = VECTOR ( 'NONE', #17485, 39.37007874015748143 ) ;
#5167 = ORIENTED_EDGE ( 'NONE', *, *, #4185, .T. ) ;
#5168 = PERSON_AND_ORGANIZATION_ROLE ( 'creator' ) ;
#5169 = CYLINDRICAL_SURFACE ( 'NONE', #18909, 1.243000000000000105 ) ;
#5170 = CARTESIAN_POINT ( 'NONE',  ( 0.000000000000000000, 5.384999999999999787, 0.000000000000000000 ) ) ;
#5171 = VERTEX_POINT ( 'NONE', #21284 ) ;
#5172 = CARTESIAN_POINT ( 'NONE',  ( 0.1292346314604057023, 0.2229166665149337201, 0.3119999999999998885 ) ) ;
#5173 = FACE_OUTER_BOUND ( 'NONE', #21031, .T. ) ;
#5174 = CARTESIAN_POINT ( 'NONE',  ( -8.964115882027956832E-07, 3.710500024236165206, -0.3119999999987121964 ) ) ;
#5175 = DIRECTION ( 'NONE',  ( -1.000000000000000000, 0.000000000000000000, 0.000000000000000000 ) ) ;
#5176 = CARTESIAN_POINT ( 'NONE',  ( 0.1419858815579627120, 0.2082143347958492208, -0.7365060972889347912 ) ) ;
#5177 = VERTEX_POINT ( 'NONE', #10198 ) ;
#5178 = ORIENTED_EDGE ( 'NONE', *, *, #7113, .T. ) ;
#5179 = DIRECTION ( 'NONE',  ( 0.8320502943378449423, -0.4803844614152608106, -0.2773500981126125753 ) ) ;
#5180 = CARTESIAN_POINT ( 'NONE',  ( 0.1954553509668046640, -0.1954553509668047195, 0.3869444444444487541 ) ) ;
#5181 = CARTESIAN_POINT ( 'NONE',  ( 0.1993543840281266633, 4.443138888964754507, -0.1993543840281266910 ) ) ;
#5182 = CARTESIAN_POINT ( 'NONE',  ( 0.3119999999999998885, 0.1812499999999996614, 0.1292346314604058410 ) ) ;
#5183 = CARTESIAN_POINT ( 'NONE',  ( 0.2464202454315519986, -0.1619151084083290393, 0.4060090615677847126 ) ) ;
#5184 = CARTESIAN_POINT ( 'NONE',  ( -0.04251946191606173486, 4.237103564431733638, 0.3090897937739507939 ) ) ;
#5185 = CARTESIAN_POINT ( 'NONE',  ( -0.1292346314604056745, 4.040361111111110404, -0.3119999999999999996 ) ) ;
#5186 = EDGE_CURVE ( 'NONE', #5448, #7946, #10080, .T. ) ;
#5187 = CARTESIAN_POINT ( 'NONE',  ( -0.3119999999999998885, 5.061194444596176290, 0.1292346314604058410 ) ) ;
#5188 = EDGE_CURVE ( 'NONE', #21090, #23820, #4576, .T. ) ;
#5189 = DIRECTION ( 'NONE',  ( 0.000000000000000000, 1.000000000000000000, 0.000000000000000000 ) ) ;
#5190 = ADVANCED_FACE ( 'NONE', ( #23093 ), #17623, .F. ) ;
#5191 = CARTESIAN_POINT ( 'NONE',  ( -0.2724990365483070387, 4.895781167980035598, 0.1573335068080851940 ) ) ;
#5192 = CONICAL_SURFACE ( 'NONE', #23878, 0.7199999999999994182, 0.7853981633974506105 ) ;
#5193 = CARTESIAN_POINT ( 'NONE',  ( -3.863846776457871776E-17, -0.3155070326520292845, 0.3574305555555597480 ) ) ;
#5194 = CARTESIAN_POINT ( 'NONE',  ( 0.1116596296178199860, 0.3830357141881718386, -0.3436530038418508792 ) ) ;
#5195 = CARTESIAN_POINT ( 'NONE',  ( 0.04345060704002973867, -0.5161796576941667380, 0.4013192973758499815 ) ) ;
#5196 = CARTESIAN_POINT ( 'NONE',  ( -0.1116596296178200276, 0.4008928570453146878, 0.3436530038418508792 ) ) ;
#5197 = CARTESIAN_POINT ( 'NONE',  ( 0.2819296736111110979, 0.3861111110352444808, -0.1167790944451422980 ) ) ;
#5198 = CARTESIAN_POINT ( 'NONE',  ( 0.1144950937579609085, -0.2764156081756484751, 0.3348611111111148841 ) ) ;
#5199 = CARTESIAN_POINT ( 'NONE',  ( 0.2819296736111110424, 5.231333333409200037, -0.1167790944451423396 ) ) ;
#5200 = CARTESIAN_POINT ( 'NONE',  ( 0.3021604925011200926, 4.472183788454629827, 0.07803024449590109657 ) ) ;
#5201 = ORIENTED_EDGE ( 'NONE', *, *, #16064, .F. ) ;
#5202 = CARTESIAN_POINT ( 'NONE',  ( -0.08088021546148146945, 3.768287267155998599, -0.3020254087663621356 ) ) ;
#5203 = CARTESIAN_POINT ( 'NONE',  ( -0.1959092998191455937, 4.605422749898409940, -0.2428318580714328434 ) ) ;
#5204 = APPROVAL ( #21156, 'UNSPECIFIED' ) ;
#5205 = CARTESIAN_POINT ( 'NONE',  ( 0.03656842479768742521, 4.876171843660301874, -0.3099543190786830937 ) ) ;
#5206 = CARTESIAN_POINT ( 'NONE',  ( 1.750236327630675475E-17, 0.05178571409062948661, -0.3999999999999999667 ) ) ;
#5207 = CARTESIAN_POINT ( 'NONE',  ( -1.910449006669871087E-17, 4.925777777777777366, -0.3119999999999999996 ) ) ;
#5208 = CARTESIAN_POINT ( 'NONE',  ( -0.2206173157302028232, 4.821611111111110404, -0.2206173157302028232 ) ) ;
#5209 = CARTESIAN_POINT ( 'NONE',  ( -0.1993543840281266910, 3.901472222298087544, -0.1993543840281266910 ) ) ;
#5210 = CARTESIAN_POINT ( 'NONE',  ( -0.1993543840281266355, 3.818138888964754507, 0.1993543840281267465 ) ) ;
#5211 = CARTESIAN_POINT ( 'NONE',  ( -0.4000000000000000222, 0.2214285714285713358, -4.898587196589413075E-17 ) ) ;
#5212 = CARTESIAN_POINT ( 'NONE',  ( 0.2206173157302028787, 4.404944444444443441, 0.2206173157302027954 ) ) ;
#5213 = ORIENTED_EDGE ( 'NONE', *, *, #7535, .F. ) ;
#5214 = CARTESIAN_POINT ( 'NONE',  ( 0.000000000000000000, 5.384999999999999787, 0.000000000000000000 ) ) ;
#5215 = CARTESIAN_POINT ( 'NONE',  ( 0.1167790944451422702, 4.446611111186975940, -0.2819296736111110424 ) ) ;
#5216 = EDGE_CURVE ( 'NONE', #11779, #6253, #10850, .T. ) ;
#5217 = CARTESIAN_POINT ( 'NONE',  ( -0.2423184047408910302, 4.508223239054410136, 0.1965347448998619739 ) ) ;
#5218 = CARTESIAN_POINT ( 'NONE',  ( 0.000000000000000000, 5.384999999999999787, 0.000000000000000000 ) ) ;
#5219 = EDGE_CURVE ( 'NONE', #4062, #9702, #1180, .T. ) ;
#5220 = CARTESIAN_POINT ( 'NONE',  ( 0.2764156081756483641, 0.1144950937579610056, 0.2306944444444475328 ) ) ;
#5221 = CARTESIAN_POINT ( 'NONE',  ( -0.1993543840281266910, 3.804250000075865668, -0.1993543840281266910 ) ) ;
#5222 = ADVANCED_FACE ( 'NONE', ( #13853 ), #11548, .T. ) ;
#5223 = CIRCLE ( 'NONE', #4828, 0.1850000000000000533 ) ;
#5224 = DIRECTION ( 'NONE',  ( 0.000000000000000000, 0.000000000000000000, -1.000000000000000000 ) ) ;
#5225 = CARTESIAN_POINT ( 'NONE',  ( -0.3120018507703757882, 4.445532957081515413, -0.04082774198810235067 ) ) ;
#5226 = CARTESIAN_POINT ( 'NONE',  ( 0.2206173157302028232, 0.07361111095937818150, -0.2206173157302028232 ) ) ;
#5227 = CARTESIAN_POINT ( 'NONE',  ( 0.2233192592356399997, 0.02232142847388616722, -0.3073725909049500049 ) ) ;
#5228 = CARTESIAN_POINT ( 'NONE',  ( 0.1167790944451423257, 0.2124999999241334314, -0.2819296736111110424 ) ) ;
#5229 = DIRECTION ( 'NONE',  ( 0.000000000000000000, 0.000000000000000000, 1.000000000000000000 ) ) ;
#5230 = CARTESIAN_POINT ( 'NONE',  ( 4.375590819076689459E-17, 0.01607142837634377430, 0.4000000000000000222 ) ) ;
#5231 = APPROVAL ( #7102, 'UNKNOWN' ) ;
#5232 = CARTESIAN_POINT ( 'NONE',  ( -0.01405487212420455066, 0.1559577530655004984, -0.7499012348325908572 ) ) ;
#5233 = CARTESIAN_POINT ( 'NONE',  ( 0.2764156081756483641, 0.1144950937579610195, 0.06402777777777945989 ) ) ;
#5234 = CARTESIAN_POINT ( 'NONE',  ( 0.2764156081756483641, -0.1144950937579611167, 0.06402777777777945989 ) ) ;
#5235 = ORIENTED_EDGE ( 'NONE', *, *, #14733, .F. ) ;
#5236 = ORIENTED_EDGE ( 'NONE', *, *, #9382, .T. ) ;
#5237 = DIRECTION ( 'NONE',  ( 0.000000000000000000, 0.000000000000000000, -1.000000000000000000 ) ) ;
#5238 = CARTESIAN_POINT ( 'NONE',  ( -0.1917383918645655105, 3.827338037112651747, -0.2494961988085758198 ) ) ;
#5239 =( GEOMETRIC_REPRESENTATION_CONTEXT ( 3 ) GLOBAL_UNCERTAINTY_ASSIGNED_CONTEXT ( ( #19473 ) ) GLOBAL_UNIT_ASSIGNED_CONTEXT ( ( #12478, #18310, #5132 ) ) REPRESENTATION_CONTEXT ( 'NONE', 'WORKASPACE' ) );
#5240 = CARTESIAN_POINT ( 'NONE',  ( -0.3119999999999999996, 0.04583333333333299009, -3.820898013339742174E-17 ) ) ;
#5241 = CARTESIAN_POINT ( 'NONE',  ( 0.1993543840281267465, 3.887583333409199149, 0.1993543840281266633 ) ) ;
#5242 = CARTESIAN_POINT ( 'NONE',  ( 0.3613381517857143232, 0.1580357141881718608, -0.1174058825155740587 ) ) ;
#5243 = ORIENTED_EDGE ( 'NONE', *, *, #89, .F. ) ;
#5244 = CARTESIAN_POINT ( 'NONE',  ( -0.2819296736111110979, 4.533416666742532186, 0.000000000000000000 ) ) ;
#5245 = DIRECTION ( 'NONE',  ( 0.000000000000000000, 1.000000000000000000, 0.000000000000000000 ) ) ;
#5246 = CARTESIAN_POINT ( 'NONE',  ( 0.000000000000000000, 1.869379215919938807E-19, -0.01219352927422984872 ) ) ;
#5247 = VERTEX_POINT ( 'NONE', #19207 ) ;
#5248 = CARTESIAN_POINT ( 'NONE',  ( 3.820898013339742174E-17, 5.384999999999999787, 0.3119999999999999996 ) ) ;
#5249 = CARTESIAN_POINT ( 'NONE',  ( 0.1751654852437733445, 4.371938874197769387, -0.2588781644951254624 ) ) ;
#5250 = CARTESIAN_POINT ( 'NONE',  ( -0.2819296736111110424, 5.134111111186975940, 0.1167790944451424923 ) ) ;
#5251 = CIRCLE ( 'NONE', #19263, 0.4000000000000000222 ) ;
#5252 = CARTESIAN_POINT ( 'NONE',  ( 7.773700634137156501E-05, 4.210497796003888737, -0.3120000004945939764 ) ) ;
#5253 = CARTESIAN_POINT ( 'NONE',  ( 1.090085390906250263E-17, 0.2805045822253778853, -1.216069878357082468 ) ) ;
#5254 = CARTESIAN_POINT ( 'NONE',  ( 0.000000000000000000, 5.384999999999999787, 0.000000000000000000 ) ) ;
#5255 = SECURITY_CLASSIFICATION ( '', '', #4212 ) ;
#5256 = CARTESIAN_POINT ( 'NONE',  ( -0.1993543840281266910, 4.901472222298087544, -0.1993543840281266910 ) ) ;
#5257 = PERSON_AND_ORGANIZATION ( #15518, #2538 ) ;
#5258 = CARTESIAN_POINT ( 'NONE',  ( -0.1670630085336562987, 4.066582461025795681, 0.2635491965915186530 ) ) ;
#5259 = CARTESIAN_POINT ( 'NONE',  ( 5.731347020009612645E-17, 4.897999999999998799, 0.3119999999999999996 ) ) ;
#5260 = ORIENTED_EDGE ( 'NONE', *, *, #7391, .T. ) ;
#5261 = CARTESIAN_POINT ( 'NONE',  ( -0.1167790944451422702, 0.2888888888130222710, -0.2819296736111110424 ) ) ;
#5262 = VERTEX_POINT ( 'NONE', #18978 ) ;
#5263 = CARTESIAN_POINT ( 'NONE',  ( 0.1167790944451423257, 0.3374999999241333204, -0.2819296736111110424 ) ) ;
#5264 = CARTESIAN_POINT ( 'NONE',  ( -0.2206173157302028232, 4.321611111111110404, -0.2206173157302028232 ) ) ;
#5265 = CARTESIAN_POINT ( 'NONE',  ( -0.1780582496145807492, 5.195124778163895840, -0.2256393913368613391 ) ) ;
#5266 = VECTOR ( 'NONE', #1523, 39.37007874015748143 ) ;
#5267 = CARTESIAN_POINT ( 'NONE',  ( 0.1236067977499789028, 0.02857142857142853584, 0.3804226065180614791 ) ) ;
#5268 = DIRECTION ( 'NONE',  ( -0.000000000000000000, 1.000000000000000000, -0.000000000000000000 ) ) ;
#5269 = EDGE_CURVE ( 'NONE', #21887, #2273, #15555, .T. ) ;
#5270 = CARTESIAN_POINT ( 'NONE',  ( 0.3119999999999999996, 4.189666666666665762, -3.820898013339742174E-17 ) ) ;
#5271 = PLANE ( 'NONE',  #11300 ) ;
#5272 = CARTESIAN_POINT ( 'NONE',  ( 0.1167790944451423257, -0.009722222298088854797, -0.2819296736111110424 ) ) ;
#5273 = CARTESIAN_POINT ( 'NONE',  ( 0.1167790944451424368, 4.550777777853644679, 0.2819296736111110424 ) ) ;
#5274 = DIRECTION ( 'NONE',  ( 0.000000000000000000, -5.763336813132313106E-16, -1.000000000000000000 ) ) ;
#5275 = CARTESIAN_POINT ( 'NONE',  ( 0.3124347497111735206, 4.530475913665126697, -0.01942892286152598721 ) ) ;
#5276 = CARTESIAN_POINT ( 'NONE',  ( -0.1167790944451423535, 4.988277777853642903, 0.2819296736111110424 ) ) ;
#5277 =( BOUNDED_SURFACE ( )  B_SPLINE_SURFACE ( 3, 2, ( 
 ( #12665, #7404, #22389 ),
 ( #19964, #12910, #14732 ),
 ( #10946, #14603, #16669 ),
 ( #20085, #20325, #22149 ),
 ( #3375, #5691, #11188 ),
 ( #1669, #75, #14481 ),
 ( #7519, #22269, #23718 ),
 ( #3613, #10827, #18373 ),
 ( #24093, #23972, #14853 ),
 ( #5567, #9101, #18137 ),
 ( #3251, #5195, #9352 ),
 ( #13031, #20447, #18254 ) ),
 .UNSPECIFIED., .F., .F., .F. ) 
 B_SPLINE_SURFACE_WITH_KNOTS ( ( 4, 2, 2, 2, 2, 4 ),
 ( 3, 3 ),
 ( 0.001926919177646337121, 0.005264799389783187192, 0.006933739495851611902, 0.008602679601920036612, 0.01194055981405688603, 0.01527844002619373545 ),
 ( 0.000000000000000000, 1.000000000000000000 ),
 .UNSPECIFIED. ) 
 GEOMETRIC_REPRESENTATION_ITEM ( )  RATIONAL_B_SPLINE_SURFACE ( (
 ( 1.000000000000000000, 0.8464669816041905381, 1.000000000000000000),
 ( 1.000000000000000000, 0.8516517675253441055, 1.000000000000000000),
 ( 1.000000000000000000, 0.8565844288627803005, 1.000000000000000000),
 ( 1.000000000000000000, 0.8620057511681040729, 1.000000000000000000),
 ( 1.000000000000000000, 0.8634777350186887412, 1.000000000000000000),
 ( 1.000000000000000000, 0.8654907715253831180, 1.000000000000000000),
 ( 1.000000000000000000, 0.8660271740516733985, 1.000000000000000000),
 ( 1.000000000000000000, 0.8660218497377574209, 1.000000000000000000),
 ( 1.000000000000000000, 0.8638283365559311644, 1.000000000000000000),
 ( 1.000000000000000000, 0.8566178551151195641, 1.000000000000000000),
 ( 1.000000000000000000, 0.8516788886408952486, 1.000000000000000000),
 ( 1.000000000000000000, 0.8464669816041903161, 1.000000000000000000) ) ) 
 REPRESENTATION_ITEM ( '' )  SURFACE ( )  );
#5278 = CARTESIAN_POINT ( 'NONE',  ( -0.2992534993645844521, 0.05134832323153658978, -0.03248684396581635186 ) ) ;
#5279 = CARTESIAN_POINT ( 'NONE',  ( 0.1736779060279114995, 3.760883958121103987, -0.2600042684560003314 ) ) ;
#5280 = LOCAL_TIME ( 21, 9, 13.00000000000000000, #6399 ) ;
#5281 = CARTESIAN_POINT ( 'NONE',  ( -5.308788303787306404E-17, 0.03949697488198145034, 0.2889969748819818385 ) ) ;
#5282 = EDGE_LOOP ( 'NONE', ( #7962, #19382, #1370, #6304 ) ) ;
#5283 = CARTESIAN_POINT ( 'NONE',  ( 4.282505654011733572E-07, 3.932722210548942776, -0.3119999999997061790 ) ) ;
#5284 = CARTESIAN_POINT ( 'NONE',  ( 0.3119999999999999996, 4.248694444596176290, 0.1292346314604056190 ) ) ;
#5285 = CARTESIAN_POINT ( 'NONE',  ( 0.1167790944451424506, 4.606333333409200037, 0.2819296736111110424 ) ) ;
#5286 = CARTESIAN_POINT ( 'NONE',  ( -0.1993543840281266910, 3.845916666742532186, -0.1993543840281266910 ) ) ;
#5287 = AXIS2_PLACEMENT_3D ( 'NONE', #22082, #3187, #16246 ) ;
#5288 = AXIS2_PLACEMENT_3D ( 'NONE', #3228, #22003, #10678 ) ;
#5289 = ORIENTED_EDGE ( 'NONE', *, *, #14382, .F. ) ;
#5290 = ADVANCED_FACE ( 'NONE', ( #2515 ), #23284, .F. ) ;
#5291 = ADVANCED_FACE ( 'NONE', ( #2276 ), #10071, .F. ) ;
#5292 = ORIENTED_EDGE ( 'NONE', *, *, #23306, .T. ) ;
#5293 = B_SPLINE_CURVE_WITH_KNOTS ( 'NONE', 3,
 ( #3507, #7295, #2412, #11930, #19349, #21177, #8239, #13523, #6175, #18994, #11440, #453, #2292, #20938, #9727, #4231, #7771, #17517, #331, #17401, #20818, #17282, #694, #11683, #18871, #6056 ),
 .UNSPECIFIED., .F., .F.,
 ( 4, 2, 2, 2, 2, 2, 2, 2, 2, 2, 2, 2, 4 ),
 ( 0.000000000000000000, 0.002376276648075994861, 0.004752553296151989723, 0.005940691620189986720, 0.007128829944227983717, 0.008316968268265981581, 0.009505106592303981181, 0.01188138324037997691, 0.01425765988845596743, 0.01544579821249396356, 0.01663393653653195969, 0.01782207486056995235, 0.01901021318460794501 ),
 .UNSPECIFIED. ) ;
#5294 = APPROVAL_STATUS ( 'not_yet_approved' ) ;
#5295 = CARTESIAN_POINT ( 'NONE',  ( -0.004657599350067381447, -0.3068592482405227972, 0.4181016929859454612 ) ) ;
#5296 = LINE ( 'NONE', #21761, #5266 ) ;
#5297 = CARTESIAN_POINT ( 'NONE',  ( -0.5116234456863258950, 1.999640111863030478, -2.727383698113316157 ) ) ;
#5298 = CC_DESIGN_APPROVAL ( #11811, ( #12722 ) ) ;
#5299 = ORIENTED_EDGE ( 'NONE', *, *, #20209, .T. ) ;
#5300 = CARTESIAN_POINT ( 'NONE',  ( 0.1292346314604057023, 0.2784722220704892726, 0.3119999999999998885 ) ) ;
#5301 = CARTESIAN_POINT ( 'NONE',  ( -0.2289623471110959485, 4.384444726759149091, -0.2119507152515421600 ) ) ;
#5302 = CARTESIAN_POINT ( 'NONE',  ( -0.1548258371540442990, 5.125004085625619155, 0.2666117704252644605 ) ) ;
#5303 = FACE_OUTER_BOUND ( 'NONE', #7127, .T. ) ;
#5304 = CARTESIAN_POINT ( 'NONE',  ( 0.1616910252715724194, 0.2282749528075390943, -0.7324324093404095404 ) ) ;
#5305 = ADVANCED_FACE ( 'NONE', ( #22978 ), #15992, .F. ) ;
#5306 = ORIENTED_EDGE ( 'NONE', *, *, #13032, .F. ) ;
#5307 = CARTESIAN_POINT ( 'NONE',  ( 0.1251933906032628718, 5.075263835759200148, 0.2864240098224283271 ) ) ;
#5308 = CARTESIAN_POINT ( 'NONE',  ( -0.1954553509668046640, 0.1954553509668046918, 0.1925000000000027245 ) ) ;
#5309 = CARTESIAN_POINT ( 'NONE',  ( -0.2819296736111110979, 4.297305555631420582, 0.000000000000000000 ) ) ;
#5310 = CARTESIAN_POINT ( 'NONE',  ( -1.726321361862525858E-17, 5.005638888964754507, -0.2819296736111110979 ) ) ;
#5311 = CARTESIAN_POINT ( 'NONE',  ( 0.1219426170921238256, -0.2560469716180380773, 0.3947246446402559727 ) ) ;
#5312 = CARTESIAN_POINT ( 'NONE',  ( -0.1515187123326594831, 4.233801538027739397, 0.2736959603349944370 ) ) ;
#5313 = CARTESIAN_POINT ( 'NONE',  ( -1.910449006669871087E-17, 3.981333333333332725, -0.3119999999999999996 ) ) ;
#5314 = CARTESIAN_POINT ( 'NONE',  ( -0.3119999999999999996, 5.057722222373953969, 0.000000000000000000 ) ) ;
#5315 = CARTESIAN_POINT ( 'NONE',  ( -1.726321361862525858E-17, 5.075083333409198261, -0.2819296736111110979 ) ) ;
#5316 = ORGANIZATION ( 'NAUO-ORG9', 'UNSPECIFIED', 'UNSPECIFIED' ) ;
#5317 = B_SPLINE_CURVE_WITH_KNOTS ( 'NONE', 3,
 ( #21217, #8043, #4270, #11845, #2451, #17204, #19262, #4386, #8161, #6336, #11972, #19386 ),
 .UNSPECIFIED., .F., .F.,
 ( 4, 2, 2, 2, 2, 4 ),
 ( 0.000000000000000000, 0.003345931539952394333, 0.005018897309928594536, 0.006691863079904794738, 0.01003779461985718734, 0.01338372615980958080 ),
 .UNSPECIFIED. ) ;
#5318 = LINE ( 'NONE', #3487, #8577 ) ;
#5319 = ORIENTED_EDGE ( 'NONE', *, *, #17365, .F. ) ;
#5320 = CARTESIAN_POINT ( 'NONE',  ( -0.1751221285957142437, 0.05731332189368815860, 0.2521211663704562289 ) ) ;
#5321 = EDGE_LOOP ( 'NONE', ( #466, #4406, #14176, #9810 ) ) ;
#5322 = CARTESIAN_POINT ( 'NONE',  ( -0.2230971623002954152, -0.2230971623002953874, 0.3504861111111152727 ) ) ;
#5323 = CARTESIAN_POINT ( 'NONE',  ( 0.1993543840281267465, 5.040361111186975940, 0.1993543840281266633 ) ) ;
#5324 = VERTEX_POINT ( 'NONE', #4930 ) ;
#5325 = CARTESIAN_POINT ( 'NONE',  ( -4.638126268221291196E-16, 0.06071428571428570675, -0.4000000000000000222 ) ) ;
#5326 = LINE ( 'NONE', #5447, #2071 ) ;
#5327 = CARTESIAN_POINT ( 'NONE',  ( -0.2819296736111110979, 0.1881944443685777957, -3.452642723725051716E-17 ) ) ;
#5328 = CARTESIAN_POINT ( 'NONE',  ( 0.2764156081756483641, -0.1144950937579611167, 0.3418055555555594704 ) ) ;
#5329 = CARTESIAN_POINT ( 'NONE',  ( 0.2819296736111110979, 5.227861111186977716, -3.452642723725051716E-17 ) ) ;
#5330 = CARTESIAN_POINT ( 'NONE',  ( 0.2961024193012317118, 4.477398186232928623, -0.1021605605434409425 ) ) ;
#5331 = VERTEX_POINT ( 'NONE', #4691 ) ;
#5332 = CARTESIAN_POINT ( 'NONE',  ( 0.2819296736111110979, 4.936194444520309865, -3.452642723725051716E-17 ) ) ;
#5333 = CARTESIAN_POINT ( 'NONE',  ( -0.3039371850020707311, 4.171187110652304852, 0.08147708232397948835 ) ) ;
#5334 = DIRECTION ( 'NONE',  ( 0.000000000000000000, 0.000000000000000000, -1.000000000000000000 ) ) ;
#5335 = CARTESIAN_POINT ( 'NONE',  ( 5.731347020009612645E-17, 4.064666666666665762, 0.3119999999999999996 ) ) ;
#5336 = CARTESIAN_POINT ( 'NONE',  ( 0.3119999999999999996, 0.5666666665149336923, 0.000000000000000000 ) ) ;
#5337 = CARTESIAN_POINT ( 'NONE',  ( 0.3119999999999999996, 4.689666666666665762, -3.820898013339742174E-17 ) ) ;
#5338 = AXIS2_PLACEMENT_3D ( 'NONE', #214, #18872, #5938 ) ;
#5339 = CARTESIAN_POINT ( 'NONE',  ( -0.2819296736111110979, 3.963972222298087544, 0.000000000000000000 ) ) ;
#5340 = CARTESIAN_POINT ( 'NONE',  ( 5.178964085587577574E-17, 3.825083333409199149, 0.2819296736111110979 ) ) ;
#5341 = CARTESIAN_POINT ( 'NONE',  ( 0.3017741391662112638, 4.032218511630571989, -0.07998161405697697124 ) ) ;
#5342 = CARTESIAN_POINT ( 'NONE',  ( 0.000000000000000000, 2.740039370078740433, -2.194053356329904947 ) ) ;
#5343 = ORIENTED_EDGE ( 'NONE', *, *, #20351, .T. ) ;
#5344 = CARTESIAN_POINT ( 'NONE',  ( 0.3119999999999999996, 3.911888888888888083, -3.820898013339742174E-17 ) ) ;
#5345 = VERTEX_POINT ( 'NONE', #14208 ) ;
#5346 = CARTESIAN_POINT ( 'NONE',  ( 0.1993543840281267465, 4.207027777853643791, 0.1993543840281266633 ) ) ;
#5347 = CARTESIAN_POINT ( 'NONE',  ( 1.241811370555571286E-09, 4.488277777895108400, -0.3119999999999999996 ) ) ;
#5348 = CARTESIAN_POINT ( 'NONE',  ( 0.1954553509668047195, 0.1954553509668046085, 0.2341666666666697150 ) ) ;
#5349 = AXIS2_PLACEMENT_3D ( 'NONE', #2906, #19979, #4732 ) ;
#5350 = CARTESIAN_POINT ( 'NONE',  ( -0.1917386117188931705, 3.954711899498488670, 0.2494960294160712411 ) ) ;
#5351 = CARTESIAN_POINT ( 'NONE',  ( -0.3038827018704687855, 4.444373711942660066, -0.08165392154346443054 ) ) ;
#5352 = EDGE_CURVE ( 'NONE', #11791, #9081, #322, .T. ) ;
#5353 = CARTESIAN_POINT ( 'NONE',  ( -0.1144950937579609918, -0.2764156081756484196, 0.3279166666666704089 ) ) ;
#5354 = CARTESIAN_POINT ( 'NONE',  ( 0.1116596296178199860, 0.2401785713310289616, -0.3436530038418508792 ) ) ;
#5355 = CARTESIAN_POINT ( 'NONE',  ( -0.2819296736111110979, 0.1743055554796889284, -3.452642723725051716E-17 ) ) ;
#5356 = CARTESIAN_POINT ( 'NONE',  ( 0.1571283209375275436, 3.853928337557731787, 0.2726217664897950255 ) ) ;
#5357 = CARTESIAN_POINT ( 'NONE',  ( 0.000000000000000000, 0.06249999999999967387, 0.000000000000000000 ) ) ;
#5358 = DIRECTION ( 'NONE',  ( -0.000000000000000000, -0.000000000000000000, -1.000000000000000000 ) ) ;
#5359 = CARTESIAN_POINT ( 'NONE',  ( 0.1144950937579609085, -0.2764156081756484751, -0.1095833333333330467 ) ) ;
#5360 = ORIENTED_EDGE ( 'NONE', *, *, #13525, .T. ) ;
#5361 = EDGE_LOOP ( 'NONE', ( #11511, #11519, #5540, #2190, #15512, #9143, #10483 ) ) ;
#5362 = CARTESIAN_POINT ( 'NONE',  ( -0.02041513420581141103, 5.092642365365469104, -0.3108785821030984886 ) ) ;
#5363 = B_SPLINE_CURVE_WITH_KNOTS ( 'NONE', 3,
 ( #3261, #1202, #6929, #23374, #1320, #12315 ),
 .UNSPECIFIED., .F., .F.,
 ( 4, 2, 4 ),
 ( 0.006804048971101872567, 0.01020032888717190694, 0.01359660880324194132 ),
 .UNSPECIFIED. ) ;
#5364 = CARTESIAN_POINT ( 'NONE',  ( 0.4687500000000002776, 0.1753644386825057300, 0.4001479654036551592 ) ) ;
#5365 = CARTESIAN_POINT ( 'NONE',  ( 0.2819296736111110424, 0.5874999999241333759, 0.1167790944451424923 ) ) ;
#5366 = CARTESIAN_POINT ( 'NONE',  ( -0.1167790944451423535, 3.766055555631421470, 0.2819296736111110424 ) ) ;
#5367 = CARTESIAN_POINT ( 'NONE',  ( -6.979263641208234666E-17, 0.2794642856167432465, 0.3799334167787516425 ) ) ;
#5368 = CARTESIAN_POINT ( 'NONE',  ( 5.178964085587577574E-17, 4.380638888964754507, 0.2819296736111110979 ) ) ;
#5369 = CARTESIAN_POINT ( 'NONE',  ( 5.731347020009612645E-17, 4.953555555555554157, 0.3119999999999999996 ) ) ;
#5370 = CARTESIAN_POINT ( 'NONE',  ( -0.3119999999999999996, 4.602861111111110404, -0.1292346314604056468 ) ) ;
#5371 = ORIENTED_EDGE ( 'NONE', *, *, #19009, .T. ) ;
#5372 = VECTOR ( 'NONE', #12083, 39.37007874015748143 ) ;
#5373 = CARTESIAN_POINT ( 'NONE',  ( 0.1919135583096156505, 4.371358422006517586, -0.2469761307552826579 ) ) ;
#5374 = CARTESIAN_POINT ( 'NONE',  ( 0.2819296736111110979, 4.877166666742533963, 0.1167790944451422425 ) ) ;
#5375 = CARTESIAN_POINT ( 'NONE',  ( 0.0005648866775877964307, 4.210483983432520283, -0.3119995209647230539 ) ) ;
#5376 = LENGTH_MEASURE_WITH_UNIT ( LENGTH_MEASURE( 0.02539999999999999897 ), #14660 );
#5377 = CARTESIAN_POINT ( 'NONE',  ( 0.4593750000000003664, 0.2760455974562901482, 0.4425000000000000044 ) ) ;
#5378 = CARTESIAN_POINT ( 'NONE',  ( 0.2472135954999579721, 0.1964285714285713969, -0.3402603233408160732 ) ) ;
#5379 = CARTESIAN_POINT ( 'NONE',  ( -0.2819296736111110979, 4.571611111186975940, -0.1167790944451422980 ) ) ;
#5380 = DATE_AND_TIME ( #23900, #21641 ) ;
#5381 = ORIENTED_EDGE ( 'NONE', *, *, #5497, .T. ) ;
#5382 = DIRECTION ( 'NONE',  ( 0.000000000000000000, 0.000000000000000000, -1.000000000000000000 ) ) ;
#5383 = CARTESIAN_POINT ( 'NONE',  ( -2.918002456435568987E-09, 4.127166543308980806, 0.3119999999999999996 ) ) ;
#5384 = CARTESIAN_POINT ( 'NONE',  ( 1.726321361862525858E-17, 0.6187499999241333759, -0.2819296736111110979 ) ) ;
#5386 = EDGE_LOOP ( 'NONE', ( #16208, #548, #5901, #12355 ) ) ;
#5385 = AXIS2_PLACEMENT_3D ( 'NONE', #21041, #4332, #11783 ) ;
#5387 = ORIENTED_EDGE ( 'NONE', *, *, #19903, .F. ) ;
#5388 = CARTESIAN_POINT ( 'NONE',  ( -0.1993543840281266633, 0.1812499999241333482, -0.1993543840281266910 ) ) ;
#5389 = DIRECTION ( 'NONE',  ( -0.3993784937532310342, 0.7060941387255963431, 0.5847460012558945985 ) ) ;
#5390 = CARTESIAN_POINT ( 'NONE',  ( -0.4116234456863466229, 1.808198851485059988, 2.607105236499406953 ) ) ;
#5391 = CARTESIAN_POINT ( 'NONE',  ( 0.1236067977499789028, -0.04285714285714287142, 0.3804226065180614791 ) ) ;
#5392 = CARTESIAN_POINT ( 'NONE',  ( -0.2230971623002953874, 0.2230971623002954152, -0.0002083333333323692741 ) ) ;
#5393 = CARTESIAN_POINT ( 'NONE',  ( 0.3860879860166717692, 1.999640111863030700, -2.647106755790660682 ) ) ;
#5394 = CARTESIAN_POINT ( 'NONE',  ( -0.5116234456863466562, 3.066692553488282957, 2.754369331946250110 ) ) ;
#5395 = CARTESIAN_POINT ( 'NONE',  ( -0.1993543840281266633, 0.1118055554796889145, -0.1993543840281266910 ) ) ;
#5396 = CARTESIAN_POINT ( 'NONE',  ( -0.1167790944451423535, 4.488277777853644679, 0.2819296736111110424 ) ) ;
#5397 = CARTESIAN_POINT ( 'NONE',  ( -7.726019084026502927E-17, 0.1589285712334866651, 0.4205848896953069405 ) ) ;
#5398 = CARTESIAN_POINT ( 'NONE',  ( 0.01388514559274585045, 4.516459957181072404, 0.3120000003946662992 ) ) ;
#5399 = CARTESIAN_POINT ( 'NONE',  ( -0.1993543840281266355, 5.040361111186977716, 0.1993543840281267465 ) ) ;
#5400 = CARTESIAN_POINT ( 'NONE',  ( 0.1993543840281267465, 4.540361111186976828, 0.1993543840281266633 ) ) ;
#5401 = EDGE_CURVE ( 'NONE', #16274, #22355, #21516, .T. ) ;
#5402 = CARTESIAN_POINT ( 'NONE',  ( 0.3120328546110059387, 4.920023481417521438, -0.04056780845644687716 ) ) ;
#5403 = FACE_OUTER_BOUND ( 'NONE', #14083, .T. ) ;
#5404 = CARTESIAN_POINT ( 'NONE',  ( 0.2191938207175568309, 3.911764414538948742, 0.2249900973144438876 ) ) ;
#5405 = CARTESIAN_POINT ( 'NONE',  ( -1.910449006669871087E-17, 4.210500000151732536, -0.3119999999999999996 ) ) ;
#5406 = CARTESIAN_POINT ( 'NONE',  ( -0.2819296736111110979, 4.477861111186976828, 0.000000000000000000 ) ) ;
#5407 = CARTESIAN_POINT ( 'NONE',  ( -0.2819296736111110424, 3.800777777853643347, 0.1167790944451424923 ) ) ;
#5408 = VECTOR ( 'NONE', #5506, 39.37007874015748143 ) ;
#5409 = VERTEX_POINT ( 'NONE', #3345 ) ;
#5410 = ADVANCED_FACE ( 'NONE', ( #18106 ), #23573, .T. ) ;
#5411 = ORIENTED_EDGE ( 'NONE', *, *, #16172, .T. ) ;
#5412 = ORIENTED_EDGE ( 'NONE', *, *, #4689, .F. ) ;
#5413 = CALENDAR_DATE ( 2026, 7, 10 ) ;
#5414 = CARTESIAN_POINT ( 'NONE',  ( -0.2980062158858403643, -0.01674720435929506757, 0.4096728825525073336 ) ) ;
#5415 = CARTESIAN_POINT ( 'NONE',  ( -1.910449006669871087E-17, 4.259111111111110404, -0.3119999999999999996 ) ) ;
#5416 = CARTESIAN_POINT ( 'NONE',  ( 0.4687500000000002776, 0.2598076211353318454, 0.3779506566538942125 ) ) ;
#5417 = EDGE_LOOP ( 'NONE', ( #11327, #17265 ) ) ;
#5418 = CARTESIAN_POINT ( 'NONE',  ( 0.2206173157302028232, 0.2958333331816003775, -0.2206173157302028232 ) ) ;
#5419 = CARTESIAN_POINT ( 'NONE',  ( -0.3125000000000000000, 0.000000000000000000, 1.326383476483184332 ) ) ;
#5420 = FACE_OUTER_BOUND ( 'NONE', #2943, .T. ) ;
#5421 = CARTESIAN_POINT ( 'NONE',  ( -0.3119999999999999996, 0.2645833333333330040, -0.1292346314604056745 ) ) ;
#5422 = DIRECTION ( 'NONE',  ( -0.8660254037844523634, -0.000000000000000000, 0.4999999999999761857 ) ) ;
#5423 =( BOUNDED_CURVE ( )  B_SPLINE_CURVE ( 2, ( #152, #7833, #2237, #2357, #5996, #2477, #9797, #22941, #17344 ),
 .UNSPECIFIED., .F., .T. ) 
 B_SPLINE_CURVE_WITH_KNOTS ( ( 3, 2, 2, 2, 3 ),
 ( 0.1979166666666667129, 0.2083333333333333703, 0.2187500000000000000, 0.2291666666666667684, 0.2395833333333334259 ),
 .UNSPECIFIED. ) 
 CURVE ( )  GEOMETRIC_REPRESENTATION_ITEM ( )  RATIONAL_B_SPLINE_CURVE ( ( 1.000000000000000222, 0.9238795325112865164, 1.000000000000000000, 0.9238795325112867385, 1.000000000000000000, 0.9238795325112867385, 1.000000000000000000, 0.9238795325112862944, 1.000000000000000444 ) ) 
 REPRESENTATION_ITEM ( '' )  );
#5424 = ORIENTED_EDGE ( 'NONE', *, *, #16191, .T. ) ;
#5425 = CARTESIAN_POINT ( 'NONE',  ( -0.2923287055106771337, 0.04017857133102904071, -0.2123892367102620804 ) ) ;
#5426 = AXIS2_PLACEMENT_3D ( 'NONE', #1049, #3447, #18209 ) ;
#5427 = ORIENTED_EDGE ( 'NONE', *, *, #467, .T. ) ;
#5428 = CARTESIAN_POINT ( 'NONE',  ( 0.2858709629710828315, 5.081892701901892018, 0.1261477422632426293 ) ) ;
#5429 = CARTESIAN_POINT ( 'NONE',  ( 0.2764156081756484196, -5.077672346800151106E-17, 0.2272222222222252119 ) ) ;
#5430 = CARTESIAN_POINT ( 'NONE',  ( 0.1993543840281266633, 4.276472222298087544, -0.1993543840281266910 ) ) ;
#5431 = CARTESIAN_POINT ( 'NONE',  ( 0.1993543840281266633, 5.165361111186976828, -0.1993543840281266910 ) ) ;
#5432 = EDGE_CURVE ( 'NONE', #9081, #21037, #22514, .T. ) ;
#5433 = DIRECTION ( 'NONE',  ( -0.000000000000000000, -1.000000000000000000, -0.000000000000000000 ) ) ;
#5434 = CARTESIAN_POINT ( 'NONE',  ( -0.3115519018914106875, 4.224912875663728862, 0.01957843891848925696 ) ) ;
#5435 = CARTESIAN_POINT ( 'NONE',  ( 0.3119999999999999996, 3.908416666666665762, 0.1292346314604056190 ) ) ;
#5436 = CARTESIAN_POINT ( 'NONE',  ( -1.910449006669871087E-17, 4.877166666818398610, -0.3119999999999999996 ) ) ;
#5437 = CARTESIAN_POINT ( 'NONE',  ( 0.1167790944451422702, 5.182722222298087544, -0.2819296736111110979 ) ) ;
#5438 = CARTESIAN_POINT ( 'NONE',  ( -0.001863919267180048824, 3.066692553488282957, 2.816660016782450704 ) ) ;
#5439 = EDGE_LOOP ( 'NONE', ( #14167, #19202, #19957, #12761 ) ) ;
#5440 = EDGE_CURVE ( 'NONE', #17116, #16274, #14089, .T. ) ;
#5441 = CARTESIAN_POINT ( 'NONE',  ( 0.01137974820294853848, 0.04292188706665825415, -0.2924218870666587256 ) ) ;
#5442 = VECTOR ( 'NONE', #1270, 39.37007874015748143 ) ;
#5443 = ORIENTED_EDGE ( 'NONE', *, *, #830, .F. ) ;
#5444 = CARTESIAN_POINT ( 'NONE',  ( -0.1306872919485615459, -0.3155070326520293400, 0.1872916666666696039 ) ) ;
#5445 = CARTESIAN_POINT ( 'NONE',  ( -0.2819296736111110424, 5.071611111186976828, -0.1167790944451423119 ) ) ;
#5446 = FACE_OUTER_BOUND ( 'NONE', #10910, .T. ) ;
#5447 = CARTESIAN_POINT ( 'NONE',  ( 0.000000000000000000, 0.000000000000000000, 0.2500000000000000000 ) ) ;
#5448 = VERTEX_POINT ( 'NONE', #1159 ) ;
#5449 = CARTESIAN_POINT ( 'NONE',  ( -0.1167790944451424506, 0.3652777777019109995, 0.2819296736111110424 ) ) ;
#5450 = CARTESIAN_POINT ( 'NONE',  ( 0.1954553509668047195, 0.1954553509668046085, 0.1855555555555581937 ) ) ;
#5451 = CARTESIAN_POINT ( 'NONE',  ( -0.1167790944451423257, 4.911888888964755395, -0.2819296736111110424 ) ) ;
#5452 = CARTESIAN_POINT ( 'NONE',  ( 0.05348210925957119777, 4.486790443027524944, -0.3073820394974481340 ) ) ;
#5453 = ORIENTED_EDGE ( 'NONE', *, *, #13328, .T. ) ;
#5454 = CARTESIAN_POINT ( 'NONE',  ( 0.1167790944451424368, 4.870222222298087544, 0.2819296736111110424 ) ) ;
#5455 = CARTESIAN_POINT ( 'NONE',  ( -0.2472135954999579444, 0.05892857123348661103, -0.3402603233408160732 ) ) ;
#5456 = VECTOR ( 'NONE', #15215, 39.37007874015748854 ) ;
#5457 = EDGE_CURVE ( 'NONE', #19011, #11232, #21879, .T. ) ;
#5458 = FACE_OUTER_BOUND ( 'NONE', #8872, .T. ) ;
#5459 = LINE ( 'NONE', #1562, #11794 ) ;
#5460 = CARTESIAN_POINT ( 'NONE',  ( -0.4620259694561524855, 0.2880908832651556950, 0.04413116910601659615 ) ) ;
#5461 = CARTESIAN_POINT ( 'NONE',  ( -0.3119999999999998885, 4.832027777777777366, 0.1292346314604058410 ) ) ;
#5462 = VECTOR ( 'NONE', #21473, 39.37007874015748143 ) ;
#5463 = ADVANCED_FACE ( 'NONE', ( #3224, #23453 ), #12396, .F. ) ;
#5464 = CARTESIAN_POINT ( 'NONE',  ( 0.2819296736111110979, 4.050777777853642903, -0.1167790944451423396 ) ) ;
#5465 = CARTESIAN_POINT ( 'NONE',  ( -0.2819296736111110979, 3.811194444520310309, 0.000000000000000000 ) ) ;
#5466 = CARTESIAN_POINT ( 'NONE',  ( 0.2223180997122823910, 4.023079565851294781, 0.2197360156277292920 ) ) ;
#5467 = CARTESIAN_POINT ( 'NONE',  ( 0.3119999999999999996, 4.411888888888888083, -3.820898013339742174E-17 ) ) ;
#5468 = VERTEX_POINT ( 'NONE', #1524 ) ;
#5469 = FACE_OUTER_BOUND ( 'NONE', #15841, .T. ) ;
#5470 = VERTEX_POINT ( 'NONE', #17990 ) ;
#5471 = CARTESIAN_POINT ( 'NONE',  ( -0.1413598573426078087, 4.122983608843597381, 0.2782734964209417350 ) ) ;
#5472 = CARTESIAN_POINT ( 'NONE',  ( -0.05455304208351747369, -0.2715891510243036988, -0.06558227484231508864 ) ) ;
#5473 = VECTOR ( 'NONE', #4012, 39.37007874015748143 ) ;
#5474 = CARTESIAN_POINT ( 'NONE',  ( 0.2764156081756484196, -5.077672346800151106E-17, 0.3383333333333372051 ) ) ;
#5475 = AXIS2_PLACEMENT_3D ( 'NONE', #6227, #21350, #19633 ) ;
#5476 = CARTESIAN_POINT ( 'NONE',  ( 0.000000000000000000, 3.738758431839877614E-19, -0.1016666666666665164 ) ) ;
#5477 = CARTESIAN_POINT ( 'NONE',  ( -0.3119981485887119987, 4.447848256106272657, 0.04085602375663895808 ) ) ;
#5478 = CARTESIAN_POINT ( 'NONE',  ( 4.589747744727345336E-07, 4.571629220806286753, 0.3119999999992840722 ) ) ;
#5479 = CARTESIAN_POINT ( 'NONE',  ( 2.326421213736078119E-17, 0.1723214284738861513, -0.3799334167787516425 ) ) ;
#5480 = CARTESIAN_POINT ( 'NONE',  ( 0.1993543840281266910, 0.1534722221463555858, -0.1993543840281266910 ) ) ;
#5481 = CARTESIAN_POINT ( 'NONE',  ( 0.01786091403636311248, 3.876684976164884056, -0.3115615677906792280 ) ) ;
#5482 = CARTESIAN_POINT ( 'NONE',  ( 3.820898013339742174E-17, 5.384999999999999787, 0.3119999999999999996 ) ) ;
#5483 = CARTESIAN_POINT ( 'NONE',  ( 0.000000000000000000, 5.384999999999999787, -0.3119999999999999996 ) ) ;
#5484 = CARTESIAN_POINT ( 'NONE',  ( -0.2764156081756484196, 0.1144950937579609918, -0.07486111111111054539 ) ) ;
#5485 = ORIENTED_EDGE ( 'NONE', *, *, #7535, .T. ) ;
#5486 = ORIENTED_EDGE ( 'NONE', *, *, #7333, .T. ) ;
#5487 = CARTESIAN_POINT ( 'NONE',  ( -0.2829274046655448904, 5.108874275092736283, 0.1269306334051448215 ) ) ;
#5488 = CARTESIAN_POINT ( 'NONE',  ( 0.3119999999999998885, 0.01458333333333300050, 0.1292346314604058410 ) ) ;
#5489 = CARTESIAN_POINT ( 'NONE',  ( 0.1993543840281266633, 3.845916666742533074, -0.1993543840281266910 ) ) ;
#5490 = CARTESIAN_POINT ( 'NONE',  ( 0.1116596296178199860, 0.2401785713310289616, -0.3436530038418508792 ) ) ;
#5491 = CARTESIAN_POINT ( 'NONE',  ( -0.2819296736111110424, 4.370222222298088433, 0.1167790944451424923 ) ) ;
#5492 = DIRECTION ( 'NONE',  ( 0.7071067811865435759, 0.000000000000000000, 0.7071067811865514585 ) ) ;
#5493 = CARTESIAN_POINT ( 'NONE',  ( 2.007333333333344516, 1.736333333333339501, -3.519666666666666721 ) ) ;
#5494 = VECTOR ( 'NONE', #9758, 39.37007874015748854 ) ;
#5495 = ORIENTED_EDGE ( 'NONE', *, *, #14837, .T. ) ;
#5496 = CARTESIAN_POINT ( 'NONE',  ( 0.2602573258582523419, 4.358078633539736124, 0.1720769237772511173 ) ) ;
#5497 = EDGE_CURVE ( 'NONE', #10448, #13469, #15350, .T. ) ;
#5498 = CARTESIAN_POINT ( 'NONE',  ( -0.1167790944451423535, 4.974388888964754507, 0.2819296736111110424 ) ) ;
#5499 = ADVANCED_FACE ( 'NONE', ( #14457 ), #13971, .T. ) ;
#5500 = CARTESIAN_POINT ( 'NONE',  ( -0.2698011859901125464, 5.151896377161309992, -0.1357330994666928470 ) ) ;
#5501 = DIRECTION ( 'NONE',  ( -1.000000000000000000, 2.385244779468088955E-18, -2.498001805406602216E-16 ) ) ;
#5502 = CARTESIAN_POINT ( 'NONE',  ( 0.8785491840485403214, 0.000000000000000000, -2.935999999999999943 ) ) ;
#5503 = CARTESIAN_POINT ( 'NONE',  ( 0.1167790944451422702, 4.668833333409200037, -0.2819296736111110979 ) ) ;
#5504 = DATE_AND_TIME ( #14420, #22039 ) ;
#5505 = CARTESIAN_POINT ( 'NONE',  ( -0.4641461581055078001, 0.2728099291808048221, 0.04698409998689238865 ) ) ;
#5506 = DIRECTION ( 'NONE',  ( -0.4999999999999913403, 0.000000000000000000, 0.8660254037844437036 ) ) ;
#5507 = CARTESIAN_POINT ( 'NONE',  ( 0.2819296736111110979, 0.5493055554796889561, 0.000000000000000000 ) ) ;
#5508 = ORIENTED_EDGE ( 'NONE', *, *, #23008, .T. ) ;
#5509 = ORIENTED_EDGE ( 'NONE', *, *, #13293, .F. ) ;
#5510 = CARTESIAN_POINT ( 'NONE',  ( 0.1993543840281266355, 0.2645833332574666907, 0.1993543840281267465 ) ) ;
#5511 = LINE ( 'NONE', #11128, #7265 ) ;
#5512 = CARTESIAN_POINT ( 'NONE',  ( 0.3950000000000000178, 0.05000000000000028727, -1.966000000000000192 ) ) ;
#5513 = CARTESIAN_POINT ( 'NONE',  ( 0.3236067977499790249, -0.02142857142857144265, -0.2351141009169892826 ) ) ;
#5514 = CARTESIAN_POINT ( 'NONE',  ( -0.2230971623002954152, -0.2230971623002953874, 0.01368055555555662377 ) ) ;
#5515 = CARTESIAN_POINT ( 'NONE',  ( -0.4206476797389064881, -0.2984048262340653901, 0.05816208736403803703 ) ) ;
#5516 = FACE_OUTER_BOUND ( 'NONE', #909, .T. ) ;
#5517 = CARTESIAN_POINT ( 'NONE',  ( -0.1167790944451424506, 0.2402777777019111383, 0.2819296736111110424 ) ) ;
#5518 = CARTESIAN_POINT ( 'NONE',  ( -0.1993543840281266633, 0.0006944443685778107491, -0.1993543840281266910 ) ) ;
#5519 = CARTESIAN_POINT ( 'NONE',  ( 5.178964085587577574E-17, 4.436194444520310753, 0.2819296736111110979 ) ) ;
#5520 = CARTESIAN_POINT ( 'NONE',  ( 0.4000000000000000222, 0.03392857123348664433, 0.000000000000000000 ) ) ;
#5521 = CARTESIAN_POINT ( 'NONE',  ( 1.995346317926969793E-07, 4.516063323326865664, 0.3119999999998666063 ) ) ;
#5522 = CARTESIAN_POINT ( 'NONE',  ( -0.2819296736111110424, 5.148000000075865223, 0.1167790944451424923 ) ) ;
#5523 = APPROVAL ( #17115, 'UNSPECIFIED' ) ;
#5524 = CARTESIAN_POINT ( 'NONE',  ( 0.2819296736111110979, 4.491750000075865223, -3.452642723725051716E-17 ) ) ;
#5525 = CYLINDRICAL_SURFACE ( 'NONE', #19984, 0.3119999999999999996 ) ;
#5526 = DIRECTION ( 'NONE',  ( 0.000000000000000000, 0.000000000000000000, 1.000000000000000000 ) ) ;
#5527 = CARTESIAN_POINT ( 'NONE',  ( 0.1195234880381787768, 3.929255801878827725, -0.2891772058695498138 ) ) ;
#5528 = CARTESIAN_POINT ( 'NONE',  ( -0.1292346314604057023, 4.012583333485065573, 0.3119999999999998885 ) ) ;
#5529 = CARTESIAN_POINT ( 'NONE',  ( 0.1167790944451424506, 4.439666666742532186, 0.2819296736111110424 ) ) ;
#5530 = CARTESIAN_POINT ( 'NONE',  ( -0.1993543840281266910, 3.790361111186976828, -0.1993543840281266910 ) ) ;
#5531 = ORIENTED_EDGE ( 'NONE', *, *, #2741, .T. ) ;
#5532 = ORIENTED_EDGE ( 'NONE', *, *, #7291, .T. ) ;
#5533 = PERSON_AND_ORGANIZATION ( #15518, #2538 ) ;
#5534 = DIRECTION ( 'NONE',  ( 0.000000000000000000, 0.000000000000000000, -1.000000000000000000 ) ) ;
#5535 = CARTESIAN_POINT ( 'NONE',  ( -0.03162305771917223868, 0.03242967361111057795, 0.2806037246084505110 ) ) ;
#5536 = PLANE ( 'NONE',  #6547 ) ;
#5537 = EDGE_CURVE ( 'NONE', #11539, #19405, #3667, .T. ) ;
#5538 = ORIENTED_EDGE ( 'NONE', *, *, #4056, .F. ) ;
#5539 = CARTESIAN_POINT ( 'NONE',  ( -5.731347020009612645E-17, 0.4416666665149336923, 0.3119999999999999996 ) ) ;
#5540 = ORIENTED_EDGE ( 'NONE', *, *, #15845, .T. ) ;
#5541 = CARTESIAN_POINT ( 'NONE',  ( 0.000000000000000000, 5.384999999999999787, 0.000000000000000000 ) ) ;
#5542 = LINE ( 'NONE', #5052, #6255 ) ;
#5543 = CARTESIAN_POINT ( 'NONE',  ( 8.375559671162349491E-15, 3.988277777929486678, -0.3119999999999999996 ) ) ;
#5544 = VERTEX_POINT ( 'NONE', #3583 ) ;
#5545 = CARTESIAN_POINT ( 'NONE',  ( -0.2233192592356400275, 0.1294642856167432798, 0.3073725909049499494 ) ) ;
#5546 = CARTESIAN_POINT ( 'NONE',  ( 0.2950997105373021068, 5.088614608052525412, -0.1005531120067661155 ) ) ;
#5547 = CARTESIAN_POINT ( 'NONE',  ( 0.000000000000000000, 0.2764156081756484196, 0.3522222222222262111 ) ) ;
#5548 = ADVANCED_FACE ( 'NONE', ( #14935 ), #9319, .T. ) ;
#5549 = CARTESIAN_POINT ( 'NONE',  ( -0.1993543840281266355, 4.193138888964754507, 0.1993543840281267465 ) ) ;
#5550 = CARTESIAN_POINT ( 'NONE',  ( -0.2819296736111110979, 5.075083333409198261, 0.000000000000000000 ) ) ;
#5551 = CARTESIAN_POINT ( 'NONE',  ( -1.910449006669871087E-17, 4.536888888888888083, -0.3119999999999999996 ) ) ;
#5552 = CARTESIAN_POINT ( 'NONE',  ( -0.2723413855784990734, 4.219733285630191233, -0.1575963679250307614 ) ) ;
#5553 = CARTESIAN_POINT ( 'NONE',  ( -0.3119999999999999996, 3.825083333333333169, -0.1292346314604056468 ) ) ;
#5554 = CARTESIAN_POINT ( 'NONE',  ( -0.3119999999999999996, 4.779944444596176290, 0.000000000000000000 ) ) ;
#5555 = VECTOR ( 'NONE', #19606, 39.37007874015748143 ) ;
#5556 = CARTESIAN_POINT ( 'NONE',  ( -0.1167790944451423119, 5.189666666742533074, -0.2819296736111110979 ) ) ;
#5557 = CARTESIAN_POINT ( 'NONE',  ( -0.1166234456863257940, 4.111524471938507119, -2.802594437230254254 ) ) ;
#5558 = CARTESIAN_POINT ( 'NONE',  ( 0.2233192592356400275, 0.2187499999024575814, -0.3073725909049499494 ) ) ;
#5559 = CARTESIAN_POINT ( 'NONE',  ( -0.4687500000000004441, 0.2922835737772480069, 0.06112444011295372487 ) ) ;
#5560 = ORIENTED_EDGE ( 'NONE', *, *, #18132, .T. ) ;
#5561 = PERSON_AND_ORGANIZATION ( #15518, #2538 ) ;
#5562 =( BOUNDED_CURVE ( )  B_SPLINE_CURVE ( 2, ( #5988, #16, #5636, #22581, #20514, #7464, #9418, #20629, #266 ),
 .UNSPECIFIED., .F., .T. ) 
 B_SPLINE_CURVE_WITH_KNOTS ( ( 3, 2, 2, 2, 3 ),
 ( 0.6145833333333333703, 0.6250000000000000000, 0.6354166666666667407, 0.6458333333333334814, 0.6562500000000001110 ),
 .UNSPECIFIED. ) 
 CURVE ( )  GEOMETRIC_REPRESENTATION_ITEM ( )  RATIONAL_B_SPLINE_CURVE ( ( 1.000000000000000000, 0.9238795325112867385, 1.000000000000000000, 0.9238795325112867385, 1.000000000000000000, 0.9238795325112867385, 1.000000000000000000, 0.9238795325112859613, 1.000000000000000888 ) ) 
 REPRESENTATION_ITEM ( '' )  );
#5563 = CARTESIAN_POINT ( 'NONE',  ( 0.2230971623002954429, 0.2230971623002953319, 0.2115972222222252952 ) ) ;
#5564 = CARTESIAN_POINT ( 'NONE',  ( 0.2819296736111110979, 5.043833333409199149, 0.1167790944451422425 ) ) ;
#5565 =( BOUNDED_CURVE ( )  B_SPLINE_CURVE ( 2, ( #21610, #18072, #2958, #17714, #4779, #10291, #6497, #6858, #10526 ),
 .UNSPECIFIED., .F., .F. ) 
 B_SPLINE_CURVE_WITH_KNOTS ( ( 3, 2, 2, 2, 3 ),
 ( 0.3958333333333333148, 0.4062500000000000000, 0.4166666666666666852, 0.4270833333333333148, 0.4375000000000000000 ),
 .UNSPECIFIED. ) 
 CURVE ( )  GEOMETRIC_REPRESENTATION_ITEM ( )  RATIONAL_B_SPLINE_CURVE ( ( 1.000000000000000000, 0.9238795325112867385, 1.000000000000000000, 0.9238795325112867385, 1.000000000000000000, 0.9238795325112867385, 1.000000000000000000, 0.9238795325112867385, 1.000000000000000000 ) ) 
 REPRESENTATION_ITEM ( '' )  );
#5566 = AXIS2_PLACEMENT_3D ( 'NONE', #11174, #10813, #20192 ) ;
#5567 = CARTESIAN_POINT ( 'NONE',  ( 0.07520958173006334069, -0.4863159908245684449, 0.4165421425001717415 ) ) ;
#5568 = CARTESIAN_POINT ( 'NONE',  ( 0.1116596296178199027, 0.3366071427596004084, 0.3436530038418508792 ) ) ;
#5569 = CARTESIAN_POINT ( 'NONE',  ( 0.2819296736111110979, 0.3826388888130222710, 0.000000000000000000 ) ) ;
#5570 = CARTESIAN_POINT ( 'NONE',  ( -0.1954553509668046918, -0.1954553509668046640, 0.2688888888888921747 ) ) ;
#5571 = CARTESIAN_POINT ( 'NONE',  ( -0.1993543840281266910, 5.026472222298088433, -0.1993543840281266910 ) ) ;
#5572 = CARTESIAN_POINT ( 'NONE',  ( 0.05322288965628670793, 4.486797450736038861, -0.3074269533229316287 ) ) ;
#5573 = EDGE_CURVE ( 'NONE', #19216, #4938, #20298, .T. ) ;
#5574 = CARTESIAN_POINT ( 'NONE',  ( -0.2819296736111110424, 4.856333333409198261, 0.1167790944451424923 ) ) ;
#5575 = DIRECTION ( 'NONE',  ( -0.8651979924482661177, 0.04370253788966847741, -0.4995222938423191095 ) ) ;
#5576 = CARTESIAN_POINT ( 'NONE',  ( 1.573500000000000343, 0.5250000000000000222, -0.5399999999999998135 ) ) ;
#5577 = LINE ( 'NONE', #16562, #6719 ) ;
#5578 = CARTESIAN_POINT ( 'NONE',  ( 0.3119999999999999996, 4.582027777777777366, -0.1292346314604056745 ) ) ;
#5579 = CARTESIAN_POINT ( 'NONE',  ( 0.1993543840281266633, 3.943138888964754507, -0.1993543840281266910 ) ) ;
#5580 = CARTESIAN_POINT ( 'NONE',  ( 0.000000000000000000, 0.000000000000000000, 1.326383476483184332 ) ) ;
#5581 = CARTESIAN_POINT ( 'NONE',  ( 0.3122779440621588076, 4.030240700459768455, -0.01080743124828337232 ) ) ;
#5582 = DIRECTION ( 'NONE',  ( 0.000000000000000000, 0.000000000000000000, -1.000000000000000000 ) ) ;
#5583 = CARTESIAN_POINT ( 'NONE',  ( 0.3120000000000000551, 3.908416666666665762, 0.1292346314604056190 ) ) ;
#5584 = ORIENTED_EDGE ( 'NONE', *, *, #21938, .T. ) ;
#5585 = AXIS2_PLACEMENT_3D ( 'NONE', #17069, #20849, #15247 ) ;
#5586 = CARTESIAN_POINT ( 'NONE',  ( -0.1022736100768033840, 4.124198058143811352, 0.2951942865389927673 ) ) ;
#5587 = CARTESIAN_POINT ( 'NONE',  ( 0.3853713378992902894, 0.3187716316911530789, 0.07807775719021836647 ) ) ;
#5588 = CARTESIAN_POINT ( 'NONE',  ( 0.03058133199899486232, 4.654066622478140403, -0.3105566612530609172 ) ) ;
#5589 = ADVANCED_FACE ( 'NONE', ( #3949 ), #5536, .F. ) ;
#5590 = CARTESIAN_POINT ( 'NONE',  ( 0.1144950937579609085, -0.2764156081756484751, 0.2168055555555584712 ) ) ;
#5591 = EDGE_CURVE ( 'NONE', #18582, #16287, #13238, .T. ) ;
#5592 = CARTESIAN_POINT ( 'NONE',  ( -5.731347020009612645E-17, 0.3930555555555551583, 0.3119999999999999996 ) ) ;
#5593 = DIRECTION ( 'NONE',  ( 0.000000000000000000, 0.000000000000000000, -1.000000000000000000 ) ) ;
#5594 = CARTESIAN_POINT ( 'NONE',  ( -0.2233192592356399997, 0.2723214284738861291, 0.3073725909049499494 ) ) ;
#5595 = CARTESIAN_POINT ( 'NONE',  ( 0.1993543840281266910, 0.2090277777019111383, -0.1993543840281266910 ) ) ;
#5596 = CARTESIAN_POINT ( 'NONE',  ( 0.04074227727064787252, 3.876059980711638264, -0.3094968829426333334 ) ) ;
#5597 = CYLINDRICAL_SURFACE ( 'NONE', #11575, 0.3125000000000000555 ) ;
#5598 = LINE ( 'NONE', #3650, #13658 ) ;
#5599 = CARTESIAN_POINT ( 'NONE',  ( 0.1144950937579611444, 0.2764156081756483641, -0.03319444444444354797 ) ) ;
#5600 = VECTOR ( 'NONE', #11738, 39.37007874015748143 ) ;
#5601 = ADVANCED_FACE ( 'NONE', ( #14702 ), #11273, .T. ) ;
#5602 = ORIENTED_EDGE ( 'NONE', *, *, #18365, .T. ) ;
#5603 = CARTESIAN_POINT ( 'NONE',  ( 0.000000000000000000, 2.735000000000000320, 0.000000000000000000 ) ) ;
#5604 = CARTESIAN_POINT ( 'NONE',  ( 0.4687500000000003331, -0.2209812308046625595, 0.4011722195456132734 ) ) ;
#5605 = CARTESIAN_POINT ( 'NONE',  ( 0.3119999999999998885, 0.07013888888888854256, 0.1292346314604058410 ) ) ;
#5606 = CARTESIAN_POINT ( 'NONE',  ( 0.3119999999999999996, 5.078555555555555046, -3.820898013339742174E-17 ) ) ;
#5607 = CARTESIAN_POINT ( 'NONE',  ( 0.3613381517857143232, 0.2258928570453146989, 0.000000000000000000 ) ) ;
#5608 = ORIENTED_EDGE ( 'NONE', *, *, #4410, .T. ) ;
#5609 = CARTESIAN_POINT ( 'NONE',  ( -0.1167790944451423257, 4.411888888964754507, -0.2819296736111110424 ) ) ;
#5610 = LINE ( 'NONE', #20490, #10053 ) ;
#5611 = CARTESIAN_POINT ( 'NONE',  ( 0.1236067977499789861, 0.4053571426620580787, -0.3804226065180614236 ) ) ;
#5612 = ORIENTED_EDGE ( 'NONE', *, *, #18696, .T. ) ;
#5613 = CARTESIAN_POINT ( 'NONE',  ( 0.2593853092514534775, 4.358033725289752525, 0.1733876775689600358 ) ) ;
#5614 = CARTESIAN_POINT ( 'NONE',  ( 5.178964085587577574E-17, 4.866750000075865223, 0.2819296736111110979 ) ) ;
#5615 = ADVANCED_FACE ( 'NONE', ( #7371 ), #12812, .T. ) ;
#5616 = PERSON ( 'NAUO-PER5', 'UNSPECIFIED', 'UNSPECIFIED', ('UNSPECIFIED'), ('UNSPECIFIED'), ('UNSPECIFIED') ) ;
#5617 = CARTESIAN_POINT ( 'NONE',  ( -0.2706342702141287804, 5.158918473216393075, 0.1307827034094938834 ) ) ;
#5618 = VECTOR ( 'NONE', #809, 39.37007874015748143 ) ;
#5619 = DIRECTION ( 'NONE',  ( 0.9999579983169535335, 0.000000000000000000, -0.009165238783119120797 ) ) ;
#5620 = DIRECTION ( 'NONE',  ( 0.8320502943378454974, -0.4803844614152598114, 0.2773500981126120757 ) ) ;
#5621 = CARTESIAN_POINT ( 'NONE',  ( -0.3119999999999998885, 4.998694444444444329, 0.1292346314604058410 ) ) ;
#5622 = CARTESIAN_POINT ( 'NONE',  ( 0.1167790944451424506, 4.592444444520309865, 0.2819296736111110424 ) ) ;
#5623 = DATE_TIME_ROLE ( 'classification_date' ) ;
#5624 = CARTESIAN_POINT ( 'NONE',  ( -0.4645997322663009688, 0.2720228281466814391, 0.05892894635879200593 ) ) ;
#5625 = LINE ( 'NONE', #16493, #21756 ) ;
#5626 = CARTESIAN_POINT ( 'NONE',  ( 0.2819296736111110424, 0.4416666665908000611, -0.1167790944451423119 ) ) ;
#5627 = ORIENTED_EDGE ( 'NONE', *, *, #12539, .T. ) ;
#5628 = VERTEX_POINT ( 'NONE', #5416 ) ;
#5629 = CARTESIAN_POINT ( 'NONE',  ( -0.2819296736111110979, 0.1881944443685777957, -3.452642723725051716E-17 ) ) ;
#5630 = ADVANCED_FACE ( 'NONE', ( #7488 ), #15057, .T. ) ;
#5631 = DIRECTION ( 'NONE',  ( 0.000000000000000000, 0.000000000000000000, -1.000000000000000000 ) ) ;
#5632 = CARTESIAN_POINT ( 'NONE',  ( -0.06335377612981453466, 0.01424091832109927562, 0.3999999999999999667 ) ) ;
#5633 = CARTESIAN_POINT ( 'NONE',  ( 0.2472135954999579721, 0.1964285714285713969, -0.3402603233408159622 ) ) ;
#5634 = CARTESIAN_POINT ( 'NONE',  ( 0.2230971623002954429, 0.2230971623002953319, -0.01409722222222137972 ) ) ;
#5635 = EDGE_CURVE ( 'NONE', #9355, #17212, #16671, .T. ) ;
#5636 = CARTESIAN_POINT ( 'NONE',  ( 0.2209708691207961095, -0.2209708691207961651, 0.03277777777777939050 ) ) ;
#5637 = CARTESIAN_POINT ( 'NONE',  ( 5.731347020009612645E-17, 4.731333333333332725, 0.3119999999999999996 ) ) ;
#5638 = CARTESIAN_POINT ( 'NONE',  ( -0.1993543840281267465, 0.2923611110352445364, 0.1993543840281266633 ) ) ;
#5639 = CARTESIAN_POINT ( 'NONE',  ( 0.2819296736111110424, 0.03194444436857781650, 0.1167790944451424923 ) ) ;
#5640 = CARTESIAN_POINT ( 'NONE',  ( 5.178964085587577574E-17, 4.547305555631421470, 0.2819296736111110979 ) ) ;
#5641 = CARTESIAN_POINT ( 'NONE',  ( -0.3236067977499789694, -0.008928571623656208003, -0.2351141009169893104 ) ) ;
#5642 = CARTESIAN_POINT ( 'NONE',  ( 0.000000000000000000, 3.669999999999999929, 0.7500000000000001110 ) ) ;
#5643 = CARTESIAN_POINT ( 'NONE',  ( -0.2819296736111110424, 5.092444444520309865, 0.1167790944451424923 ) ) ;
#5644 = CARTESIAN_POINT ( 'NONE',  ( 0.2819296736111111534, 4.488277777853643791, 0.1167790944451422563 ) ) ;
#5645 = CARTESIAN_POINT ( 'NONE',  ( 0.3119669420168502683, 4.917723305947723667, 0.04107160245604204313 ) ) ;
#5646 = CARTESIAN_POINT ( 'NONE',  ( -0.3146277125502374705, 0.3722332453489713422, 0.07156651416104445329 ) ) ;
#5647 = CARTESIAN_POINT ( 'NONE',  ( 0.3119999999999999996, 3.974388889040620931, -3.820898013339742174E-17 ) ) ;
#5648 = LOCAL_TIME ( 21, 9, 13.00000000000000000, #733 ) ;
#5649 = DIRECTION ( 'NONE',  ( -0.8660254037844526964, 0.000000000000000000, 0.4999999999999756306 ) ) ;
#5650 = ORIENTED_EDGE ( 'NONE', *, *, #2163, .T. ) ;
#5651 = CARTESIAN_POINT ( 'NONE',  ( -0.4366234456863467006, 0.9548081934128058723, 2.592671479769666387 ) ) ;
#5652 = EDGE_LOOP ( 'NONE', ( #13403, #22438, #12834, #21050 ) ) ;
#5653 = ORIENTED_EDGE ( 'NONE', *, *, #6637, .T. ) ;
#5654 = PERSON_AND_ORGANIZATION ( #15518, #2538 ) ;
#5655 = CARTESIAN_POINT ( 'NONE',  ( -1.910449006669871087E-17, 4.259111111111110404, -0.3119999999999999996 ) ) ;
#5656 = VECTOR ( 'NONE', #10671, 39.37007874015748143 ) ;
#5657 = CARTESIAN_POINT ( 'NONE',  ( -0.1341874927019925390, 4.845446088247941319, 0.2816776366694470068 ) ) ;
#5658 = CARTESIAN_POINT ( 'NONE',  ( 1.020000000000000018, 2.665000000000000036, -2.591000000000000192 ) ) ;
#5659 = ORIENTED_EDGE ( 'NONE', *, *, #9519, .T. ) ;
#5660 = CARTESIAN_POINT ( 'NONE',  ( -0.2206173157302028787, 0.4902777776260447973, 0.2206173157302027954 ) ) ;
#5661 = VERTEX_POINT ( 'NONE', #18704 ) ;
#5662 = DIRECTION ( 'NONE',  ( 0.000000000000000000, 0.000000000000000000, 1.000000000000000000 ) ) ;
#5663 = CARTESIAN_POINT ( 'NONE',  ( 0.2136809747524369418, 4.759464567214101827, -0.2316255526684406485 ) ) ;
#5664 = CARTESIAN_POINT ( 'NONE',  ( 0.2233192592356399164, 0.05446428561674330343, 0.3073725909049500604 ) ) ;
#5665 = CARTESIAN_POINT ( 'NONE',  ( 0.1570236185076638036, 3.965114079239589362, 0.2726776789891453556 ) ) ;
#5666 = ORIENTED_EDGE ( 'NONE', *, *, #19549, .T. ) ;
#5667 = SECURITY_CLASSIFICATION ( '', '', #19445 ) ;
#5668 = CARTESIAN_POINT ( 'NONE',  ( -0.2923287055106771337, 0.1830357141881718552, -0.2123892367102620804 ) ) ;
#5669 = CARTESIAN_POINT ( 'NONE',  ( 0.1311029671040783717, 5.096026576386377904, -0.2823468851309067773 ) ) ;
#5670 = CARTESIAN_POINT ( 'NONE',  ( -0.2969103764849149174, 4.671736745946869718, 0.09797322420413220878 ) ) ;
#5671 = CARTESIAN_POINT ( 'NONE',  ( 0.1993543840281267465, 4.151472222298087544, 0.1993543840281266633 ) ) ;
#5672 = CARTESIAN_POINT ( 'NONE',  ( -0.2819296736111110979, 5.130638888964754507, 0.000000000000000000 ) ) ;
#5673 = CARTESIAN_POINT ( 'NONE',  ( 0.3006586688675964014, -0.04349558104366376549, 0.4153305990016259441 ) ) ;
#5674 = CARTESIAN_POINT ( 'NONE',  ( 1.020000000000000018, 0.000000000000000000, -2.540999999999999925 ) ) ;
#5675 = CARTESIAN_POINT ( 'NONE',  ( 0.3119999999999999996, 3.911888888888888083, -3.820898013339742174E-17 ) ) ;
#5676 = CARTESIAN_POINT ( 'NONE',  ( -0.3119999999999999996, 4.835500000151732536, 0.000000000000000000 ) ) ;
#5677 = CARTESIAN_POINT ( 'NONE',  ( 0.3104765647686094643, 4.806875790144055749, 0.03085341637652804989 ) ) ;
#5678 = EDGE_CURVE ( 'NONE', #14932, #14671, #19786, .T. ) ;
#5679 = CARTESIAN_POINT ( 'NONE',  ( 0.3119999999999998885, 0.4034722222222218435, 0.1292346314604058410 ) ) ;
#5680 = ORIENTED_EDGE ( 'NONE', *, *, #6985, .F. ) ;
#5681 = CARTESIAN_POINT ( 'NONE',  ( 0.2923287055106771337, 0.07232142847388615958, -0.2123892367102620249 ) ) ;
#5682 = APPROVAL_PERSON_ORGANIZATION ( #16370, #3454, #8925 ) ;
#5683 = CARTESIAN_POINT ( 'NONE',  ( 0.2568083155295264319, 0.03694455021989599686, -0.1289653288417937083 ) ) ;
#5684 = ORIENTED_EDGE ( 'NONE', *, *, #17942, .F. ) ;
#5685 = PERSON_AND_ORGANIZATION_ROLE ( 'creator' ) ;
#5686 = CC_DESIGN_DATE_AND_TIME_ASSIGNMENT ( #5504, #3189, ( #4895 ) ) ;
#5687 = FACE_OUTER_BOUND ( 'NONE', #4305, .T. ) ;
#5688 = CARTESIAN_POINT ( 'NONE',  ( 0.1993543840281267465, 5.207027777853642903, 0.1993543840281266633 ) ) ;
#5689 = CARTESIAN_POINT ( 'NONE',  ( -0.1167790944451423119, 3.911888888964754507, -0.2819296736111110979 ) ) ;
#5690 = AXIS2_PLACEMENT_3D ( 'NONE', #7691, #4271, #20736 ) ;
#5691 = CARTESIAN_POINT ( 'NONE',  ( 0.3118573088780851599, -0.3612149761357442146, 0.4243809486557439392 ) ) ;
#5692 = DIRECTION ( 'NONE',  ( -1.000000000000000000, 0.000000000000000000, 0.000000000000000000 ) ) ;
#5693 = CARTESIAN_POINT ( 'NONE',  ( 0.1954553509668046640, -0.1954553509668047195, -0.001944444444443294917 ) ) ;
#5694 = CARTESIAN_POINT ( 'NONE',  ( -0.1993543840281267465, 0.5840277777019110550, 0.1993543840281266633 ) ) ;
#5695 = CARTESIAN_POINT ( 'NONE',  ( 0.1144950937579611444, 0.2764156081756483641, 0.3001388888888924522 ) ) ;
#5696 = CARTESIAN_POINT ( 'NONE',  ( -0.2819296736111110424, 4.981333333409199149, 0.1167790944451424923 ) ) ;
#5697 = CARTESIAN_POINT ( 'NONE',  ( -0.1292346314604081170, 3.929249999999999687, -0.3119999999999975016 ) ) ;
#5698 = CARTESIAN_POINT ( 'NONE',  ( -0.1993543840281266910, 4.845916666742532186, -0.1993543840281266910 ) ) ;
#5699 = CARTESIAN_POINT ( 'NONE',  ( -0.1236067977499790416, 0.08392857123348662629, 0.3804226065180614236 ) ) ;
#5700 = CARTESIAN_POINT ( 'NONE',  ( -1.858121103377620624E-07, 4.877166671810766019, -0.3119999999999446549 ) ) ;
#5701 = DIRECTION ( 'NONE',  ( -0.000000000000000000, -1.000000000000000000, -0.000000000000000000 ) ) ;
#5702 = CARTESIAN_POINT ( 'NONE',  ( 2.064333333333333353, 0.8966666666666665009, 0.8466666666666669006 ) ) ;
#5703 = ADVANCED_FACE ( 'NONE', ( #1878 ), #14575, .F. ) ;
#5704 = CARTESIAN_POINT ( 'NONE',  ( 0.1292346314604058410, 4.568138888888888971, 0.3119999999999998885 ) ) ;
#5705 = CARTESIAN_POINT ( 'NONE',  ( 0.1993543840281266633, 3.887583333409198705, -0.1993543840281266910 ) ) ;
#5706 = CARTESIAN_POINT ( 'NONE',  ( 1.573500000000000343, -3.414809992080329023E-17, -1.412500000000000089 ) ) ;
#5707 = CARTESIAN_POINT ( 'NONE',  ( 0.1951823636048612975, 4.022064155229219118, 0.2434209937556025827 ) ) ;
#5708 = CARTESIAN_POINT ( 'NONE',  ( -0.09974310894697509255, 3.735413644336969430, 0.2956453992739275227 ) ) ;
#5709 = VECTOR ( 'NONE', #8684, 39.37007874015748143 ) ;
#5710 = CARTESIAN_POINT ( 'NONE',  ( 0.1540770959472501922, 4.594794592340397443, -0.2743014874479684506 ) ) ;
#5711 = VERTEX_POINT ( 'NONE', #2003 ) ;
#5712 = EDGE_CURVE ( 'NONE', #3971, #11248, #20537, .T. ) ;
#5713 =( BOUNDED_CURVE ( )  B_SPLINE_CURVE ( 2, ( #9716, #5925, #2161, #2519, #6163, #802, #5807, #9961, #21046 ),
 .UNSPECIFIED., .F., .T. ) 
 B_SPLINE_CURVE_WITH_KNOTS ( ( 3, 2, 2, 2, 3 ),
 ( 0.2053571428571429325, 0.2098214285714285754, 0.2142857142857141906, 0.2187499999999998335, 0.2232142857142854764 ),
 .UNSPECIFIED. ) 
 CURVE ( )  GEOMETRIC_REPRESENTATION_ITEM ( )  RATIONAL_B_SPLINE_CURVE ( ( 0.9999999999999985567, 0.9238795325112881818, 1.000000000000000000, 0.9238795325112867385, 1.000000000000000000, 0.9238795325112867385, 1.000000000000000000, 0.9238795325112909573, 0.9999999999999957812 ) ) 
 REPRESENTATION_ITEM ( '' )  );
#5714 =( BOUNDED_CURVE ( )  B_SPLINE_CURVE ( 2, ( #13431, #2209, #22439, #15017, #365, #7807, #20852, #4143, #2326, #17200, #13313, #485, #13558 ),
 .UNSPECIFIED., .F., .F. ) 
 B_SPLINE_CURVE_WITH_KNOTS ( ( 3, 2, 2, 2, 2, 2, 3 ),
 ( 0.6785714285714286031, 0.6857142857142857206, 0.6999999999999999556, 0.7142857142857143016, 0.7285714285714285365, 0.7428571428571428825, 0.7500000000000000000 ),
 .UNSPECIFIED. ) 
 CURVE ( )  GEOMETRIC_REPRESENTATION_ITEM ( )  RATIONAL_B_SPLINE_CURVE ( ( 0.9755282581475768211, 0.9755282581475769321, 1.000000000000000000, 0.9510565162951535312, 1.000000000000000000, 0.9510565162951535312, 1.000000000000000000, 0.9510565162951535312, 1.000000000000000000, 0.9510565162951535312, 1.000000000000000000, 0.9755282581475768211, 0.9755282581475768211 ) ) 
 REPRESENTATION_ITEM ( '' )  );
#5715 = CARTESIAN_POINT ( 'NONE',  ( 2.725416254512337932, 2.978485840173427324, -2.591000000000000636 ) ) ;
#5716 = EDGE_CURVE ( 'NONE', #7699, #18597, #16875, .T. ) ;
#5717 = CARTESIAN_POINT ( 'NONE',  ( 0.1303732590071332853, 4.151117928182491035, -0.2856235017375695628 ) ) ;
#5718 = CARTESIAN_POINT ( 'NONE',  ( -0.2764156081756484196, -0.1144950937579609362, 0.4251388888888933959 ) ) ;
#5719 = CARTESIAN_POINT ( 'NONE',  ( 0.1900105704308386045, 5.206640035683666845, 0.2082794372640154323 ) ) ;
#5720 = CARTESIAN_POINT ( 'NONE',  ( 0.3008229147836520290, 5.144663873052548908, 0.04257211586236403500 ) ) ;
#5721 = ORIENTED_EDGE ( 'NONE', *, *, #20732, .F. ) ;
#5722 = CARTESIAN_POINT ( 'NONE',  ( -0.2923287055106771337, 0.2544642856167432798, -0.2123892367102620804 ) ) ;
#5723 = CIRCLE ( 'NONE', #1814, 0.4453125000000000000 ) ;
#5724 = CARTESIAN_POINT ( 'NONE',  ( -0.1993543840281266633, 0.1673611110352444808, -0.1993543840281266910 ) ) ;
#5725 = DIRECTION ( 'NONE',  ( 0.000000000000000000, 0.000000000000000000, 1.000000000000000000 ) ) ;
#5726 = CARTESIAN_POINT ( 'NONE',  ( 0.2674045363888666316, 0.6373041478666018333, -1.088102446297350534 ) ) ;
#5727 = CARTESIAN_POINT ( 'NONE',  ( 0.000000000000000000, 5.384999999999999787, 0.000000000000000000 ) ) ;
#5728 = CARTESIAN_POINT ( 'NONE',  ( -0.1954553509668046918, -0.1954553509668046640, -0.06444444444444380471 ) ) ;
#5729 = CARTESIAN_POINT ( 'NONE',  ( -0.01015435915181665469, 5.092370350171590232, -0.3113982329504829671 ) ) ;
#5730 = CARTESIAN_POINT ( 'NONE',  ( 0.4593405033095763201, 0.04515253527788225252, 0.4334345840242775361 ) ) ;
#5731 = CARTESIAN_POINT ( 'NONE',  ( 0.2206173157302028232, 0.3027777777777774237, -0.2206173157302028232 ) ) ;
#5732 = CARTESIAN_POINT ( 'NONE',  ( -0.1292346314604057023, 5.227861111111110404, 0.3119999999999998885 ) ) ;
#5733 = EDGE_LOOP ( 'NONE', ( #1881, #2952, #21768, #17828 ) ) ;
#5734 = CARTESIAN_POINT ( 'NONE',  ( 0.1993543840281267465, 4.276472222298088433, 0.1993543840281266633 ) ) ;
#5735 = FACE_OUTER_BOUND ( 'NONE', #13772, .T. ) ;
#5736 = CARTESIAN_POINT ( 'NONE',  ( -0.4116234456863256952, 2.853030769935287037, -2.698516184653834582 ) ) ;
#5737 = ADVANCED_FACE ( 'NONE', ( #21998 ), #1515, .T. ) ;
#5738 = ORIENTED_EDGE ( 'NONE', *, *, #23208, .T. ) ;
#5739 = EDGE_CURVE ( 'NONE', #6274, #1526, #6265, .T. ) ;
#5740 = CARTESIAN_POINT ( 'NONE',  ( -0.2819296736111110424, 4.960500000075865223, -0.1167790944451423119 ) ) ;
#5741 = DIRECTION ( 'NONE',  ( 0.000000000000000000, 0.000000000000000000, 1.000000000000000000 ) ) ;
#5742 = AXIS2_PLACEMENT_3D ( 'NONE', #17970, #3205, #1383 ) ;
#5743 = EDGE_CURVE ( 'NONE', #10641, #6836, #2370, .T. ) ;
#5744 =( CONVERSION_BASED_UNIT ( 'INCH', #7690 ) LENGTH_UNIT ( ) NAMED_UNIT ( #11808 ) );
#5745 = CARTESIAN_POINT ( 'NONE',  ( -0.09435543239135868454, 3.514980167629567998, 2.763260016782451700 ) ) ;
#5746 = CARTESIAN_POINT ( 'NONE',  ( -0.2819296736111110424, 4.745222222298088433, 0.1167790944451424923 ) ) ;
#5747 = APPROVAL_DATE_TIME ( #3918, #12871 ) ;
#5748 = CARTESIAN_POINT ( 'NONE',  ( -0.1530498720672202884, 4.067052562292516882, 0.2718834723444233381 ) ) ;
#5749 = CARTESIAN_POINT ( 'NONE',  ( -0.1144950937579609918, -0.2764156081756484196, 0.05013888888889046075 ) ) ;
#5750 = CARTESIAN_POINT ( 'NONE',  ( 0.1993543840281266355, 0.5423611110352445364, 0.1993543840281267465 ) ) ;
#5751 = ORIENTED_EDGE ( 'NONE', *, *, #12124, .T. ) ;
#5752 = VERTEX_POINT ( 'NONE', #2247 ) ;
#5753 = CARTESIAN_POINT ( 'NONE',  ( 0.2819296736111110979, 0.2159722221463555858, 0.000000000000000000 ) ) ;
#5754 = DIRECTION ( 'NONE',  ( 1.000000000000000000, 0.000000000000000000, 0.000000000000000000 ) ) ;
#5755 = CARTESIAN_POINT ( 'NONE',  ( 0.3125000000000000000, -5.740531871003217465E-17, 0.1994444444444470055 ) ) ;
#5756 = CARTESIAN_POINT ( 'NONE',  ( -0.3236067977499790249, 0.2999999999999999334, 0.2351141009169892271 ) ) ;
#5757 = CARTESIAN_POINT ( 'NONE',  ( 0.1306872919485616846, 0.3155070326520292290, -0.06618055555555513170 ) ) ;
#5758 = CARTESIAN_POINT ( 'NONE',  ( -0.08494034609768597033, -0.4922255456807479446, 0.06591861138174437418 ) ) ;
#5759 = CARTESIAN_POINT ( 'NONE',  ( -0.2800968539712042626, 1.715098578335394762E-17, -0.06926352063787094560 ) ) ;
#5760 = CARTESIAN_POINT ( 'NONE',  ( -0.2819296736111110979, 0.3409722221463556413, -3.452642723725051716E-17 ) ) ;
#5761 = CARTESIAN_POINT ( 'NONE',  ( 1.079423153357894183, 2.439495096761426396, -1.077972490201325906 ) ) ;
#5762 = CARTESIAN_POINT ( 'NONE',  ( 0.1993543840281266633, 4.179250000075865223, -0.1993543840281266910 ) ) ;
#5763 = AXIS2_PLACEMENT_3D ( 'NONE', #18777, #14247, #12836 ) ;
#5764 = CARTESIAN_POINT ( 'NONE',  ( -7.726019084026502927E-17, 0.01607142837634378124, 0.4205848896953069405 ) ) ;
#5765 = CARTESIAN_POINT ( 'NONE',  ( 0.1167790944451424368, 4.773000000075866112, 0.2819296736111110424 ) ) ;
#5766 = CARTESIAN_POINT ( 'NONE',  ( 5.178964085587577574E-17, 4.366750000075866112, 0.2819296736111110979 ) ) ;
#5767 = CARTESIAN_POINT ( 'NONE',  ( -0.001863919267180048824, 3.514980167629567998, 2.816660016782450704 ) ) ;
#5768 = CARTESIAN_POINT ( 'NONE',  ( 0.3135651898165193185, 3.919649592934535853, -0.02960734467547308443 ) ) ;
#5769 = CARTESIAN_POINT ( 'NONE',  ( -0.3119999999999999996, 4.168833333485065573, 0.000000000000000000 ) ) ;
#5770 = CARTESIAN_POINT ( 'NONE',  ( -0.4000000000000000222, 0.2874999998049151406, 0.1299678784931624920 ) ) ;
#5771 = CARTESIAN_POINT ( 'NONE',  ( -0.1111235690147887867, -0.2883545979861809605, -0.09773750720628669730 ) ) ;
#5772 = ORIENTED_EDGE ( 'NONE', *, *, #5088, .F. ) ;
#5773 = VECTOR ( 'NONE', #9489, 39.37007874015748143 ) ;
#5774 = CALENDAR_DATE ( 2026, 7, 10 ) ;
#5775 = CARTESIAN_POINT ( 'NONE',  ( 1.972716373660570399, 2.672602470488781190, -2.673753908138122526 ) ) ;
#5776 = CARTESIAN_POINT ( 'NONE',  ( -0.5116234456863258950, 1.658283848634127366, -2.715836692729523438 ) ) ;
#5777 = ORIENTED_EDGE ( 'NONE', *, *, #10985, .T. ) ;
#5778 = CARTESIAN_POINT ( 'NONE',  ( 1.910449006669871087E-17, 0.4694444442927115380, -0.3119999999999999996 ) ) ;
#5779 = ORIENTED_EDGE ( 'NONE', *, *, #8881, .F. ) ;
#5780 = FACE_OUTER_BOUND ( 'NONE', #19468, .T. ) ;
#5781 = FACE_OUTER_BOUND ( 'NONE', #15701, .T. ) ;
#5782 = CARTESIAN_POINT ( 'NONE',  ( -0.3613381517857143232, -0.04196428581182810175, -4.425116109941954795E-17 ) ) ;
#5783 = DIRECTION ( 'NONE',  ( -0.000000000000000000, 1.000000000000000000, -0.000000000000000000 ) ) ;
#5784 = ORIENTED_EDGE ( 'NONE', *, *, #20361, .T. ) ;
#5785 = CARTESIAN_POINT ( 'NONE',  ( -0.3613381517857143788, 0.1937499999024576425, 0.1174058825155740310 ) ) ;
#5786 = LINE ( 'NONE', #11528, #1776 ) ;
#5787 = CARTESIAN_POINT ( 'NONE',  ( 0.2764156081756483641, 0.1144950937579610056, 0.3973611111111154393 ) ) ;
#5788 = CARTESIAN_POINT ( 'NONE',  ( -0.1167790944451423257, 3.953555555631421914, -0.2819296736111110424 ) ) ;
#5789 = CARTESIAN_POINT ( 'NONE',  ( 0.01388454463234072185, 5.043460286985110841, -0.3120000000000000551 ) ) ;
#5790 = FACE_BOUND ( 'NONE', #2668, .T. ) ;
#5791 = CARTESIAN_POINT ( 'NONE',  ( 0.2206173157302028787, 3.849388888888888083, 0.2206173157302027954 ) ) ;
#5792 = AXIS2_PLACEMENT_3D ( 'NONE', #21374, #12133, #1009 ) ;
#5793 = CARTESIAN_POINT ( 'NONE',  ( -0.3119999999999998885, 4.672305555707288782, 0.1292346314604058410 ) ) ;
#5794 = CARTESIAN_POINT ( 'NONE',  ( -0.1993543840281266355, 5.151472222298088433, 0.1993543840281267465 ) ) ;
#5795 = CARTESIAN_POINT ( 'NONE',  ( -0.1167790944451423257, 4.175777777853643791, -0.2819296736111110424 ) ) ;
#5796 = CARTESIAN_POINT ( 'NONE',  ( -0.06721871850921422309, 3.903017741005486485, 0.3063181425897485433 ) ) ;
#5797 = VERTEX_POINT ( 'NONE', #19421 ) ;
#5798 = EDGE_CURVE ( 'NONE', #14944, #3503, #19737, .T. ) ;
#5799 = CARTESIAN_POINT ( 'NONE',  ( 0.3613381517857143232, 0.2044642856167432909, 0.1174058825155741975 ) ) ;
#5800 = ORIENTED_EDGE ( 'NONE', *, *, #8889, .F. ) ;
#5801 = PERSON_AND_ORGANIZATION_ROLE ( 'design_supplier' ) ;
#5802 = CARTESIAN_POINT ( 'NONE',  ( 0.4593750000000003664, 0.2760455974562900372, 0.06112444011295369711 ) ) ;
#5803 = CARTESIAN_POINT ( 'NONE',  ( 0.2819296736111110424, 5.161888888964753619, -0.1167790944451423396 ) ) ;
#5804 = CARTESIAN_POINT ( 'NONE',  ( 0.1167790944451422702, 3.793833333409199149, -0.2819296736111110979 ) ) ;
#5805 = VECTOR ( 'NONE', #19436, 39.37007874015748143 ) ;
#5806 = CARTESIAN_POINT ( 'NONE',  ( 0.2211792888862010864, 4.425861817871897586, -0.2225068856345374380 ) ) ;
#5807 = CARTESIAN_POINT ( 'NONE',  ( -0.2206173157302028232, 4.932722222222221120, -0.2206173157302028232 ) ) ;
#5808 = CARTESIAN_POINT ( 'NONE',  ( 0.000000000000000000, 0.2764156081756484196, 0.1855555555555581937 ) ) ;
#5809 = CARTESIAN_POINT ( 'NONE',  ( -0.1993543840281267465, 0.5284722221463555858, 0.1993543840281266633 ) ) ;
#5810 = CARTESIAN_POINT ( 'NONE',  ( -0.1144950937579609918, -0.2764156081756484196, 0.4390277777777824020 ) ) ;
#5811 = CARTESIAN_POINT ( 'NONE',  ( -0.2819296736111110424, 4.863277777853643791, -0.1167790944451423119 ) ) ;
#5812 = CARTESIAN_POINT ( 'NONE',  ( 0.2727366458256587634, 4.469775673605889565, 0.1569361545628811805 ) ) ;
#5813 = CARTESIAN_POINT ( 'NONE',  ( 0.1993543840281267465, 4.818138888964754507, 0.1993543840281266633 ) ) ;
#5814 = DIRECTION ( 'NONE',  ( 0.8660254037844361541, 0.000000000000000000, 0.5000000000000042188 ) ) ;
#5815 = CARTESIAN_POINT ( 'NONE',  ( 0.3125000000000000000, -5.740531871003217465E-17, 0.3661111111111149397 ) ) ;
#5816 = CARTESIAN_POINT ( 'NONE',  ( 0.3120000000000000551, 4.075083333333332725, 0.1292346314604056190 ) ) ;
#5817 = DIRECTION ( 'NONE',  ( 0.03777542905056541916, -0.9971419496943164651, 0.06542896239329260011 ) ) ;
#5818 = CARTESIAN_POINT ( 'NONE',  ( 0.2206173157302027954, 4.418833333333332725, -0.2206173157302028232 ) ) ;
#5819 = CARTESIAN_POINT ( 'NONE',  ( -0.1236067977499790416, 0.3071428571428570509, 0.3804226065180614236 ) ) ;
#5820 = PLANE ( 'NONE',  #6186 ) ;
#5821 = CYLINDRICAL_SURFACE ( 'NONE', #18618, 0.3119999999999999996 ) ;
#5822 = CC_DESIGN_PERSON_AND_ORGANIZATION_ASSIGNMENT ( #20441, #23626, ( #11902 ) ) ;
#5823 = DIRECTION ( 'NONE',  ( 0.5589148618992055839, 0.8148277346686835232, -0.1538503817443866439 ) ) ;
#5824 = TOROIDAL_SURFACE ( 'NONE', #23713, -0.5601250000000235207, 1.200750000000023521 ) ;
#5825 = CARTESIAN_POINT ( 'NONE',  ( -1.910449006669871087E-17, 4.536888888888888083, -0.3119999999999999996 ) ) ;
#5826 = B_SPLINE_CURVE_WITH_KNOTS ( 'NONE', 3,
 ( #20475, #21815, #3280, #16338, #23750, #12696, #21930, #3405, #10855, #13297, #15559, #2633, #6405, #18889, #11456, #2750, #12038, #11333, #5831, #10321, #18762, #22543, #20711, #21162, #2189, #5720, #14997, #17054, #9621, #6284, #13739, #10082, #17503, #4007, #19337, #21287, #4453, #13180, #347, #17746, #7786, #15797, #22980, #15677, #11917, #23217 ),
 .UNSPECIFIED., .F., .F.,
 ( 4, 2, 2, 2, 2, 2, 2, 2, 2, 2, 2, 2, 2, 2, 2, 2, 2, 2, 2, 2, 2, 2, 4 ),
 ( 0.02876147360672271294, 0.02951887419360549672, 0.03027627478048828050, 0.03179107595425384458, 0.03330587712801941214, 0.03406327771490218898, 0.03482067830178496581, 0.03633547947555052643, 0.03785028064931608704, 0.03936508182308164072, 0.04012248240996442450, 0.04087988299684719440, 0.04163728358372997818, 0.04239468417061275501, 0.04390948534437830869, 0.04542428651814386931, 0.04693908769190942298, 0.04769648827879220676, 0.04845388886567497666, 0.04996869003944054421, 0.05148349121320609789, 0.05224089180008888167, 0.05299829238697165851 ),
 .UNSPECIFIED. ) ;
#5827 = VERTEX_POINT ( 'NONE', #23425 ) ;
#5828 = CARTESIAN_POINT ( 'NONE',  ( -0.1656294416274741443, 4.122187037343969074, 0.2644585830901644008 ) ) ;
#5829 = CARTESIAN_POINT ( 'NONE',  ( -0.2764156081756484196, -0.1144950937579609362, 0.3695833333333374826 ) ) ;
#5830 = CARTESIAN_POINT ( 'NONE',  ( 0.04084089659891350366, 4.320441687794666308, -0.3120000000710619892 ) ) ;
#5831 = CARTESIAN_POINT ( 'NONE',  ( 0.2937600628871613329, 5.148624849934147818, -0.07568332425666259022 ) ) ;
#5832 = ORIENTED_EDGE ( 'NONE', *, *, #21809, .F. ) ;
#5833 = AXIS2_PLACEMENT_3D ( 'NONE', #7666, #17626, #20592 ) ;
#5834 = ADVANCED_FACE ( 'NONE', ( #21491 ), #886, .T. ) ;
#5835 = CARTESIAN_POINT ( 'NONE',  ( 0.3613381517857143232, 0.3008928570453147100, -0.1174058825155740587 ) ) ;
#5836 = VECTOR ( 'NONE', #10461, 39.37007874015748143 ) ;
#5837 = CARTESIAN_POINT ( 'NONE',  ( 0.1993543840281266355, 0.5284722221463555858, 0.1993543840281267465 ) ) ;
#5838 = CARTESIAN_POINT ( 'NONE',  ( 0.000000000000000000, 0.2764156081756484196, -0.1408333333333332826 ) ) ;
#5839 = CARTESIAN_POINT ( 'NONE',  ( 0.1923949478952308167, 0.2387739693004125863, -1.212204774773908866 ) ) ;
#5840 = CARTESIAN_POINT ( 'NONE',  ( 0.1584465904743050102, 0.4497866957027559787, 0.4135550951626319471 ) ) ;
#5841 = CARTESIAN_POINT ( 'NONE',  ( -0.1144950937579609779, 0.2764156081756484196, 0.1959722222222249899 ) ) ;
#5842 = LINE ( 'NONE', #13305, #537 ) ;
#5843 = CARTESIAN_POINT ( 'NONE',  ( 0.06335377612981431261, 0.1213837754639564281, -0.4000000000000000777 ) ) ;
#5844 = CARTESIAN_POINT ( 'NONE',  ( -0.2206173157302027954, 0.3166666666666663188, -0.2206173157302028232 ) ) ;
#5845 = CARTESIAN_POINT ( 'NONE',  ( -0.1292346314604056745, 5.262583333333332725, -0.3119999999999999996 ) ) ;
#5846 = EDGE_CURVE ( 'NONE', #21247, #10793, #5565, .T. ) ;
#5847 = CARTESIAN_POINT ( 'NONE',  ( -1.726321361862525858E-17, 4.186194444520309865, -0.2819296736111110979 ) ) ;
#5848 = CARTESIAN_POINT ( 'NONE',  ( -0.4366234456863259394, 1.999640111863030478, -2.684082427924094016 ) ) ;
#5849 = CARTESIAN_POINT ( 'NONE',  ( 0.3999999999999999667, 0.3946428569477721804, -0.1299678784931625197 ) ) ;
#5850 = ORIENTED_EDGE ( 'NONE', *, *, #13080, .F. ) ;
#5851 = EDGE_LOOP ( 'NONE', ( #13655, #10913, #18380, #20492 ) ) ;
#5852 = CARTESIAN_POINT ( 'NONE',  ( 0.1292346314604056745, 0.3618055555555552694, -0.3119999999999999996 ) ) ;
#5853 = CARTESIAN_POINT ( 'NONE',  ( -1.726321361862525858E-17, 4.894527777853642903, -0.2819296736111110979 ) ) ;
#5854 = AXIS2_PLACEMENT_3D ( 'NONE', #7529, #14864, #11074 ) ;
#5855 = CARTESIAN_POINT ( 'NONE',  ( -0.09684493161512809645, 5.145868290167153525, -0.2881700814494116969 ) ) ;
#5856 = DIRECTION ( 'NONE',  ( -0.8371691043312236014, 0.000000000000000000, -0.5469441386039866071 ) ) ;
#5857 = DIRECTION ( 'NONE',  ( 0.8660254037844434816, 0.000000000000000000, 0.4999999999999916178 ) ) ;
#5858 = CARTESIAN_POINT ( 'NONE',  ( -0.1144950937579609779, 0.2764156081756484196, -0.1443055555555555203 ) ) ;
#5859 = CARTESIAN_POINT ( 'NONE',  ( 0.1167790944451424506, 4.759111111186976828, 0.2819296736111110424 ) ) ;
#5860 = CARTESIAN_POINT ( 'NONE',  ( 5.731347020009612645E-17, 4.286888888888888083, 0.3119999999999999996 ) ) ;
#5861 = CARTESIAN_POINT ( 'NONE',  ( -0.1954553509668046640, 0.1954553509668046918, -0.02277777777777679341 ) ) ;
#5862 = CARTESIAN_POINT ( 'NONE',  ( 0.2819296736111110424, 0.6013888888130223265, 0.1167790944451424923 ) ) ;
#5863 = ORIENTED_EDGE ( 'NONE', *, *, #16177, .F. ) ;
#5864 = CARTESIAN_POINT ( 'NONE',  ( 0.1993543840281266355, 0.4312499999241333759, 0.1993543840281267465 ) ) ;
#5865 = DIRECTION ( 'NONE',  ( 0.000000000000000000, 0.000000000000000000, 1.000000000000000000 ) ) ;
#5866 = CARTESIAN_POINT ( 'NONE',  ( 0.7108475124358174524, 3.066692553488282957, 2.927961747820534644 ) ) ;
#5867 = CARTESIAN_POINT ( 'NONE',  ( 0.2472135954999579166, 0.1749999999999999889, 0.3402603233408160732 ) ) ;
#5868 = CARTESIAN_POINT ( 'NONE',  ( 0.3155070326520292290, 0.1306872919485615736, 0.09354166666666836882 ) ) ;
#5869 = CARTESIAN_POINT ( 'NONE',  ( -0.2819296736111110979, 0.2263888888130222710, -0.1167790944451423396 ) ) ;
#5870 = CARTESIAN_POINT ( 'NONE',  ( 1.726321361862525858E-17, 0.2159722221463555858, -0.2819296736111110979 ) ) ;
#5871 = VERTEX_POINT ( 'NONE', #10416 ) ;
#5872 = AXIS2_PLACEMENT_3D ( 'NONE', #22226, #482, #5526 ) ;
#5873 = CARTESIAN_POINT ( 'NONE',  ( 5.178964085587577574E-17, 4.380638888964754507, 0.2819296736111110979 ) ) ;
#5874 = CARTESIAN_POINT ( 'NONE',  ( -0.2472135954999579999, 0.1517857140906294644, 0.3402603233408159622 ) ) ;
#5875 = EDGE_CURVE ( 'NONE', #6276, #10051, #17325, .T. ) ;
#5876 = CARTESIAN_POINT ( 'NONE',  ( -0.2819296736111110424, 4.918833333409199149, -0.1167790944451423119 ) ) ;
#5877 = CARTESIAN_POINT ( 'NONE',  ( 0.2819296736111110979, 4.436194444520309865, -3.452642723725051716E-17 ) ) ;
#5878 = CARTESIAN_POINT ( 'NONE',  ( 7.484242640931070629E-07, 4.016084960865516251, 0.3119999999981048489 ) ) ;
#5879 = CARTESIAN_POINT ( 'NONE',  ( -0.2209708691207961095, 0.2209708691207961373, 0.1091666666666684937 ) ) ;
#5880 = CARTESIAN_POINT ( 'NONE',  ( -0.3119999999999999996, 4.165361111262843252, -0.1292346314604056468 ) ) ;
#5881 = LINE ( 'NONE', #2241, #6789 ) ;
#5882 = DIRECTION ( 'NONE',  ( -0.000000000000000000, -1.000000000000000000, -0.000000000000000000 ) ) ;
#5883 = ORIENTED_EDGE ( 'NONE', *, *, #3136, .T. ) ;
#5884 = VECTOR ( 'NONE', #9444, 39.37007874015748143 ) ;
#5885 = APPROVAL_STATUS ( 'not_yet_approved' ) ;
#5886 = VERTEX_POINT ( 'NONE', #14424 ) ;
#5887 = CARTESIAN_POINT ( 'NONE',  ( 0.2525416622817170942, 0.1285646679930055047, 0.3944156602770289566 ) ) ;
#5888 = LINE ( 'NONE', #20649, #586 ) ;
#5889 = ADVANCED_FACE ( 'NONE', ( #10172 ), #13944, .F. ) ;
#5890 = CARTESIAN_POINT ( 'NONE',  ( -0.3866234456863258395, 3.706421428007538488, -2.712949941383575592 ) ) ;
#5891 = ORIENTED_EDGE ( 'NONE', *, *, #8761, .T. ) ;
#5892 = CARTESIAN_POINT ( 'NONE',  ( 0.2206173157302028232, 0.5736111109593782231, -0.2206173157302028232 ) ) ;
#5893 = EDGE_CURVE ( 'NONE', #20052, #21090, #8439, .T. ) ;
#5894 = ADVANCED_FACE ( 'NONE', ( #11004 ), #1490, .F. ) ;
#5895 = ORIENTED_EDGE ( 'NONE', *, *, #1659, .F. ) ;
#5896 = CARTESIAN_POINT ( 'NONE',  ( 0.3253415854805812857, 4.021672897201586740E-17, -0.1145082521472477743 ) ) ;
#5897 = CARTESIAN_POINT ( 'NONE',  ( 0.1504789989860620958, 0.4433647533406533392, 0.4295860435587880999 ) ) ;
#5898 = DIRECTION ( 'NONE',  ( 1.000000000000000000, 0.000000000000000000, 0.000000000000000000 ) ) ;
#5899 = CARTESIAN_POINT ( 'NONE',  ( 0.3613381517857143232, 0.06517857133102902822, 0.000000000000000000 ) ) ;
#5900 = CARTESIAN_POINT ( 'NONE',  ( -0.1292346314604056190, 0.4798611111111107941, -0.3119999999999999996 ) ) ;
#5901 = ORIENTED_EDGE ( 'NONE', *, *, #15732, .F. ) ;
#5902 = CARTESIAN_POINT ( 'NONE',  ( 0.1116596296178199027, 0.2830357141881718053, 0.3436530038418508792 ) ) ;
#5903 = VERTEX_POINT ( 'NONE', #7577 ) ;
#5904 = CARTESIAN_POINT ( 'NONE',  ( 1.910449006669871087E-17, 0.2472222220704892726, -0.3119999999999999996 ) ) ;
#5905 = CARTESIAN_POINT ( 'NONE',  ( 0.1144950937579611444, 0.2764156081756483641, 0.4598611111111159389 ) ) ;
#5906 = EDGE_CURVE ( 'NONE', #544, #21142, #10769, .T. ) ;
#5907 = CARTESIAN_POINT ( 'NONE',  ( -0.1993543840281266355, 4.082027777853643791, 0.1993543840281267465 ) ) ;
#5908 = CARTESIAN_POINT ( 'NONE',  ( 2.936000000000000387, 0.000000000000000000, -0.04999999999999918399 ) ) ;
#5909 = CARTESIAN_POINT ( 'NONE',  ( -0.2206173157302027676, 4.835499999999999687, 0.2206173157302028787 ) ) ;
#5910 = CARTESIAN_POINT ( 'NONE',  ( -0.1292346314604056745, 3.762583333333332725, -0.3119999999999999996 ) ) ;
#5911 = CARTESIAN_POINT ( 'NONE',  ( 0.1292346314604058410, 4.797305555707287894, 0.3119999999999998885 ) ) ;
#5912 = CARTESIAN_POINT ( 'NONE',  ( 0.2819296736111111534, 4.946611111186976828, 0.1167790944451422563 ) ) ;
#5913 = ORIENTED_EDGE ( 'NONE', *, *, #2897, .T. ) ;
#5914 = CARTESIAN_POINT ( 'NONE',  ( 5.178964085587577574E-17, 4.366750000075866112, 0.2819296736111110979 ) ) ;
#5915 = CARTESIAN_POINT ( 'NONE',  ( 0.2233192592356399164, 0.05446428561674330343, 0.3073725909049500604 ) ) ;
#5916 = VERTEX_POINT ( 'NONE', #1727 ) ;
#5917 = VERTEX_POINT ( 'NONE', #12730 ) ;
#5918 = B_SPLINE_CURVE_WITH_KNOTS ( 'NONE', 3,
 ( #6697, #12555, #7175, #8748, #10715, #8878, #14494, #12416, #6788, #11476, #1959, #8980 ),
 .UNSPECIFIED., .F., .F.,
 ( 4, 2, 2, 2, 2, 4 ),
 ( 0.000000000000000000, 0.001334276959395565938, 0.002668553918791131876, 0.004002830878186698464, 0.004669969357884482843, 0.005337107837582267221 ),
 .UNSPECIFIED. ) ;
#5919 = DATE_AND_TIME ( #11665, #19293 ) ;
#5920 = CARTESIAN_POINT ( 'NONE',  ( 0.000000000000000000, 6.000000000000000888, -0.2041999999999999926 ) ) ;
#5921 = DIRECTION ( 'NONE',  ( 0.000000000000000000, -0.9961946980917454342, -0.08715574274765833240 ) ) ;
#5922 = CARTESIAN_POINT ( 'NONE',  ( 0.2819296736111110979, 3.898000000075866112, -0.1167790944451423396 ) ) ;
#5923 = CARTESIAN_POINT ( 'NONE',  ( -0.02441201398334205686, 3.066692553488282957, 3.451468604327566858 ) ) ;
#5924 = CARTESIAN_POINT ( 'NONE',  ( 0.003269416932269875696, -0.5491886443627421732, 0.04193793378272824696 ) ) ;
#5925 = CARTESIAN_POINT ( 'NONE',  ( -0.1292346314604075619, 4.950083333333332725, 0.3119999999999980567 ) ) ;
#5926 = CARTESIAN_POINT ( 'NONE',  ( 0.1954553509668046640, -0.1954553509668047195, 0.2202777777777807366 ) ) ;
#5927 = CARTESIAN_POINT ( 'NONE',  ( 0.1993543840281266355, 0.4868055554796889561, 0.1993543840281267465 ) ) ;
#5928 = CARTESIAN_POINT ( 'NONE',  ( -0.1144950937579609779, 0.2764156081756484196, 0.4737500000000048894 ) ) ;
#5929 = EDGE_CURVE ( 'NONE', #3340, #16124, #22371, .T. ) ;
#5930 = CARTESIAN_POINT ( 'NONE',  ( 0.1167790944451422702, 4.960500000075865223, -0.2819296736111110424 ) ) ;
#5931 = DIRECTION ( 'NONE',  ( -0.3535533905932684018, -0.7071067811865462405, -0.6123724356957992443 ) ) ;
#5932 = AXIS2_PLACEMENT_3D ( 'NONE', #13752, #19222, #11800 ) ;
#5933 = EDGE_CURVE ( 'NONE', #5247, #1426, #21371, .T. ) ;
#5934 = CARTESIAN_POINT ( 'NONE',  ( 0.1167790944451422702, 4.557722222298087544, -0.2819296736111110424 ) ) ;
#5935 = CARTESIAN_POINT ( 'NONE',  ( 4.589422455927707524E-07, 4.793851445074613693, 0.3119999999992840167 ) ) ;
#5936 = CARTESIAN_POINT ( 'NONE',  ( 0.2122804003021576125, 4.856019927748675968, 0.2286534880123932689 ) ) ;
#5937 = PLANE ( 'NONE',  #3219 ) ;
#5938 = DIRECTION ( 'NONE',  ( 0.000000000000000000, 0.000000000000000000, 1.000000000000000000 ) ) ;
#5939 = CARTESIAN_POINT ( 'NONE',  ( -0.3119999999999999996, 4.436194444444444329, -0.1292346314604056468 ) ) ;
#5940 = CARTESIAN_POINT ( 'NONE',  ( 0.2819296736111111534, 3.877166666742532186, 0.1167790944451422563 ) ) ;
#5941 = LINE ( 'NONE', #4113, #10484 ) ;
#5942 = CARTESIAN_POINT ( 'NONE',  ( -0.2206173157302027676, 4.002166666666665762, 0.2206173157302028787 ) ) ;
#5943 = VERTEX_POINT ( 'NONE', #18432 ) ;
#5944 = CARTESIAN_POINT ( 'NONE',  ( 0.3117100783463861990, 4.585130279527236397, 0.01372980001063455260 ) ) ;
#5945 = ORIENTED_EDGE ( 'NONE', *, *, #19344, .T. ) ;
#5946 = CARTESIAN_POINT ( 'NONE',  ( -0.2348293880619035656, 4.119665766202905033, 0.2088470014844988898 ) ) ;
#5947 = CONICAL_SURFACE ( 'NONE', #17633, 0.1874999999999998335, 1.029744258676652757 ) ;
#5948 = DIRECTION ( 'NONE',  ( -0.000000000000000000, 1.000000000000000000, -0.000000000000000000 ) ) ;
#5949 = CARTESIAN_POINT ( 'NONE',  ( 0.1306872919485614071, -0.3155070326520293955, -0.08354166666666594521 ) ) ;
#5950 = DIRECTION ( 'NONE',  ( 0.000000000000000000, 0.000000000000000000, 1.000000000000000000 ) ) ;
#5951 = EDGE_LOOP ( 'NONE', ( #18918, #18174, #5800, #8437 ) ) ;
#5952 = CARTESIAN_POINT ( 'NONE',  ( 0.2923287055106771337, 0.0008928570453147542749, -0.2123892367102620249 ) ) ;
#5953 = CARTESIAN_POINT ( 'NONE',  ( -0.1167790944451424368, 0.4624999999241333759, 0.2819296736111110424 ) ) ;
#5954 = DIRECTION ( 'NONE',  ( -0.000000000000000000, -1.000000000000000000, -0.000000000000000000 ) ) ;
#5955 = DIRECTION ( 'NONE',  ( -0.5773502691896299499, 0.5773502691896236216, -0.5773502691896236216 ) ) ;
#5956 = CARTESIAN_POINT ( 'NONE',  ( -0.1144950937579609779, 0.2764156081756484196, 0.1404166666666689378 ) ) ;
#5957 = B_SPLINE_CURVE_WITH_KNOTS ( 'NONE', 3,
 ( #12819, #11092, #12572, #5924, #18981, #22058, #1811, #20115 ),
 .UNSPECIFIED., .F., .F.,
 ( 4, 2, 2, 4 ),
 ( 0.000000000000000000, 0.0004997454757086389372, 0.0007496182135629584058, 0.0009994909514172778744 ),
 .UNSPECIFIED. ) ;
#5958 = CARTESIAN_POINT ( 'NONE',  ( -0.3078280617541462316, 4.614801766752763434, 0.05510150218785365983 ) ) ;
#5959 = CARTESIAN_POINT ( 'NONE',  ( -0.3616234456863257618, 4.559812086079793048, -2.727383698113316157 ) ) ;
#5960 = CARTESIAN_POINT ( 'NONE',  ( 0.3119999999999999996, 0.2958333333333329485, 0.000000000000000000 ) ) ;
#5961 = CARTESIAN_POINT ( 'NONE',  ( -0.3119999999999998885, 5.220916666666665762, 0.1292346314604058410 ) ) ;
#5962 = AXIS2_PLACEMENT_3D ( 'NONE', #3866, #1789, #22150 ) ;
#5963 = CARTESIAN_POINT ( 'NONE',  ( -0.1167790944451423257, 4.245222222298088433, -0.2819296736111110424 ) ) ;
#5964 = PLANE ( 'NONE',  #6538 ) ;
#5965 = LINE ( 'NONE', #11025, #429 ) ;
#5966 = DIRECTION ( 'NONE',  ( -0.4999999999999942268, 0.000000000000000000, 0.8660254037844420383 ) ) ;
#5967 = VERTEX_POINT ( 'NONE', #14669 ) ;
#5968 = CARTESIAN_POINT ( 'NONE',  ( 0.3119999999999999996, 0.3513888888888885287, 0.000000000000000000 ) ) ;
#5969 = CARTESIAN_POINT ( 'NONE',  ( 0.1993543840281267465, 4.762583333409199149, 0.1993543840281266633 ) ) ;
#5970 = CARTESIAN_POINT ( 'NONE',  ( 0.2923287055106771337, 0.3580357141881718164, -0.2123892367102620249 ) ) ;
#5971 = EDGE_CURVE ( 'NONE', #13964, #7602, #4925, .T. ) ;
#5972 = CARTESIAN_POINT ( 'NONE',  ( -0.2387229431459631235, 5.150382089001773522, -0.1856462434723448740 ) ) ;
#5973 = DIRECTION ( 'NONE',  ( 1.000000000000000000, 0.000000000000000000, 0.000000000000000000 ) ) ;
#5974 = CARTESIAN_POINT ( 'NONE',  ( 0.04478946178605012346, 3.709278574126537276, -0.3088990676013957937 ) ) ;
#5975 = CARTESIAN_POINT ( 'NONE',  ( 2.325416254512337577, 2.978485840173427324, -2.591000000000000636 ) ) ;
#5976 = CARTESIAN_POINT ( 'NONE',  ( -1.726321361862525858E-17, 4.408416666742533074, -0.2819296736111110979 ) ) ;
#5977 = SECURITY_CLASSIFICATION_LEVEL ( 'unclassified' ) ;
#5978 = VECTOR ( 'NONE', #13101, 39.37007874015748143 ) ;
#5979 = CARTESIAN_POINT ( 'NONE',  ( -0.02226417865471658208, 4.044440256128997824, -0.3112113514703778727 ) ) ;
#5980 = CARTESIAN_POINT ( 'NONE',  ( 0.2764156081756483641, 0.1144950937579610195, 0.01541666666666794208 ) ) ;
#5981 = CARTESIAN_POINT ( 'NONE',  ( 1.750236327630675475E-17, 0.2749999999999999112, -0.3999999999999999667 ) ) ;
#5982 = ORIENTED_EDGE ( 'NONE', *, *, #7369, .F. ) ;
#5983 = CARTESIAN_POINT ( 'NONE',  ( -0.2819296736111110424, 0.4624999999241333759, -0.1167790944451423396 ) ) ;
#5984 = FACE_OUTER_BOUND ( 'NONE', #6690, .T. ) ;
#5985 = CARTESIAN_POINT ( 'NONE',  ( -0.3999999999999999667, 0.3517857140906294200, -0.1299678784931626030 ) ) ;
#5986 = CARTESIAN_POINT ( 'NONE',  ( -0.3999999999999999667, 0.2178571428571427493, -0.1299678784931626030 ) ) ;
#5987 = CARTESIAN_POINT ( 'NONE',  ( 0.000000000000000000, 0.3155070326520292845, 0.2706250000000031131 ) ) ;
#5988 = CARTESIAN_POINT ( 'NONE',  ( 0.3125000000000000000, -5.740531871003217465E-17, 0.03972222222222387966 ) ) ;
#5989 = LINE ( 'NONE', #504, #5050 ) ;
#5990 = CARTESIAN_POINT ( 'NONE',  ( 0.2819296736111110424, 0.4763888888130222710, 0.1167790944451424923 ) ) ;
#5991 = CARTESIAN_POINT ( 'NONE',  ( 0.2819296736111110424, 0.2611111110352444808, -0.1167790944451423119 ) ) ;
#5992 = CARTESIAN_POINT ( 'NONE',  ( -0.1993543840281266355, 4.262583333409199149, 0.1993543840281267465 ) ) ;
#5993 = CARTESIAN_POINT ( 'NONE',  ( -0.3999999999999999667, 0.4232142855192008724, -0.1299678784931626030 ) ) ;
#5994 = CARTESIAN_POINT ( 'NONE',  ( -0.2819296736111110979, 4.866750000075866112, 0.000000000000000000 ) ) ;
#5995 = CARTESIAN_POINT ( 'NONE',  ( -0.2819296736111110979, 4.182722222298087544, -0.1167790944451422980 ) ) ;
#5996 = CARTESIAN_POINT ( 'NONE',  ( -3.827021247335479543E-17, -0.3125000000000000000, 0.3036111111111148841 ) ) ;
#5997 = ORIENTED_EDGE ( 'NONE', *, *, #8670, .F. ) ;
#5998 = CARTESIAN_POINT ( 'NONE',  ( -0.009375000000000069042, 0.5358532185916218271, 0.06112444011295372487 ) ) ;
#5999 = CARTESIAN_POINT ( 'NONE',  ( -1.910449006669871087E-17, 3.988277777929510215, -0.3119999999999999996 ) ) ;
#6000 = CARTESIAN_POINT ( 'NONE',  ( 0.000000000000000000, 0.4199999999999998734, 0.000000000000000000 ) ) ;
#6001 = ORIENTED_EDGE ( 'NONE', *, *, #17678, .T. ) ;
#6002 = AXIS2_PLACEMENT_3D ( 'NONE', #7571, #16721, #13436 ) ;
#6003 = COORDINATED_UNIVERSAL_TIME_OFFSET ( 0, 0, .AHEAD. ) ;
#6004 = ADVANCED_FACE ( 'NONE', ( #15025 ), #9284, .T. ) ;
#6005 = CARTESIAN_POINT ( 'NONE',  ( 0.1236067977499789861, 0.3428571428571428048, -0.3804226065180614236 ) ) ;
#6006 =( BOUNDED_CURVE ( )  B_SPLINE_CURVE ( 2, ( #15364, #13779, #21207, #4499, #11964, #246, #19135, #15130, #20967 ),
 .UNSPECIFIED., .F., .F. ) 
 B_SPLINE_CURVE_WITH_KNOTS ( ( 3, 2, 2, 2, 3 ),
 ( 0.9196428571428570953, 0.9241071428571429047, 0.9285714285714286031, 0.9330357142857144126, 0.9375000000000001110 ),
 .UNSPECIFIED. ) 
 CURVE ( )  GEOMETRIC_REPRESENTATION_ITEM ( )  RATIONAL_B_SPLINE_CURVE ( ( 1.000000000000000000, 0.9238795325112867385, 1.000000000000000000, 0.9238795325112867385, 1.000000000000000000, 0.9238795325112867385, 1.000000000000000000, 0.9238795325112848511, 1.000000000000001998 ) ) 
 REPRESENTATION_ITEM ( '' )  );
#6007 = DIRECTION ( 'NONE',  ( -1.000000000000000000, 0.000000000000000000, 0.000000000000000000 ) ) ;
#6008 = CARTESIAN_POINT ( 'NONE',  ( -0.2447671590917250006, 5.008122686144473867, 0.1936521771237534884 ) ) ;
#6009 = VERTEX_POINT ( 'NONE', #20385 ) ;
#6010 = CARTESIAN_POINT ( 'NONE',  ( 0.2206173157302028232, 0.4069444442927114824, -0.2206173157302028232 ) ) ;
#6011 = ORIENTED_EDGE ( 'NONE', *, *, #21933, .F. ) ;
#6012 = CARTESIAN_POINT ( 'NONE',  ( -0.4749999999999999778, 3.575000000000000622, -0.09499999999999995948 ) ) ;
#6013 = CARTESIAN_POINT ( 'NONE',  ( 0.1557525356064934918, 0.4513421090059003271, 0.4242370903632993739 ) ) ;
#6014 = CARTESIAN_POINT ( 'NONE',  ( -0.2206173157302028787, 0.5527777777777773682, 0.2206173157302027954 ) ) ;
#6015 = CARTESIAN_POINT ( 'NONE',  ( 0.1116596296178199027, 0.05089285704531473081, 0.3436530038418508792 ) ) ;
#6016 = CARTESIAN_POINT ( 'NONE',  ( -1.399103805173478513E-17, 0.4635611116728546865, -1.084197934689580034 ) ) ;
#6017 = ORIENTED_EDGE ( 'NONE', *, *, #11879, .T. ) ;
#6018 = CARTESIAN_POINT ( 'NONE',  ( 0.2233192592356399164, 0.3580357141881718164, 0.3073725909049500604 ) ) ;
#6019 = FACE_OUTER_BOUND ( 'NONE', #2864, .T. ) ;
#6020 = CARTESIAN_POINT ( 'NONE',  ( -8.252060436089559755E-07, 4.682689096385127314, 0.3119999999976427185 ) ) ;
#6021 = CARTESIAN_POINT ( 'NONE',  ( -0.1167790944451423535, 3.918833333409198705, 0.2819296736111110424 ) ) ;
#6022 = DIRECTION ( 'NONE',  ( 0.000000000000000000, 0.000000000000000000, 1.000000000000000000 ) ) ;
#6023 = CARTESIAN_POINT ( 'NONE',  ( 0.07921175570129510013, 5.120394104548939396, 0.2987029092252261320 ) ) ;
#6024 = LOCAL_TIME ( 21, 9, 13.00000000000000000, #16214 ) ;
#6025 = CARTESIAN_POINT ( 'NONE',  ( -0.2896199013420221458, 5.181292007268502253, 0.04275989185916429652 ) ) ;
#6026 = CARTESIAN_POINT ( 'NONE',  ( 0.3119999999999999996, 4.637583333485064685, 0.1292346314604056190 ) ) ;
#6027 = CARTESIAN_POINT ( 'NONE',  ( 0.2819296736111110979, 4.953555555631421470, -0.1167790944451423396 ) ) ;
#6028 = ORIENTED_EDGE ( 'NONE', *, *, #3668, .F. ) ;
#6029 = EDGE_CURVE ( 'NONE', #22719, #16231, #22148, .T. ) ;
#6030 = ADVANCED_FACE ( 'NONE', ( #16847 ), #16727, .F. ) ;
#6031 = CARTESIAN_POINT ( 'NONE',  ( -0.2819296736111110424, 4.238277777853642903, -0.1167790944451423119 ) ) ;
#6032 = EDGE_CURVE ( 'NONE', #10685, #11161, #12603, .T. ) ;
#6033 = ORIENTED_EDGE ( 'NONE', *, *, #1536, .F. ) ;
#6034 = CONICAL_SURFACE ( 'NONE', #3706, 0.6391249999999999432, 1.134464013796309345 ) ;
#6035 = ORIENTED_EDGE ( 'NONE', *, *, #14007, .F. ) ;
#6036 = ORIENTED_EDGE ( 'NONE', *, *, #4978, .F. ) ;
#6037 = PERSON_AND_ORGANIZATION ( #15518, #2538 ) ;
#6038 = EDGE_CURVE ( 'NONE', #9585, #21966, #5625, .T. ) ;
#6039 = CARTESIAN_POINT ( 'NONE',  ( -0.2230971623002953874, 0.2230971623002954152, 0.3921527777777822354 ) ) ;
#6040 = CARTESIAN_POINT ( 'NONE',  ( 1.109470958122167561, 2.291712385858714285, -1.012998853824579992 ) ) ;
#6041 = LOCAL_TIME ( 21, 9, 13.00000000000000000, #6640 ) ;
#6042 = CARTESIAN_POINT ( 'NONE',  ( 5.178964085587577574E-17, 3.880638888964754951, 0.2819296736111110979 ) ) ;
#6043 = CARTESIAN_POINT ( 'NONE',  ( 0.2988699043018692714, 4.421723770119410979, -0.09822243194017121759 ) ) ;
#6044 = CARTESIAN_POINT ( 'NONE',  ( 0.1292346314604045920, 4.623694444444444329, 0.3120000000000012208 ) ) ;
#6045 = CARTESIAN_POINT ( 'NONE',  ( 0.4570242136016807177, -0.2774028246161671651, 0.04874733047933994118 ) ) ;
#6046 = CARTESIAN_POINT ( 'NONE',  ( 0.2764156081756483641, -0.1144950937579611028, 0.2237500000000029743 ) ) ;
#6047 = CARTESIAN_POINT ( 'NONE',  ( 0.1167790944451423119, 0.5041666665908001166, -0.2819296736111110979 ) ) ;
#6048 = CARTESIAN_POINT ( 'NONE',  ( 0.1144950937579611444, 0.2764156081756483641, 0.4112500000000043898 ) ) ;
#6049 = VERTEX_POINT ( 'NONE', #12848 ) ;
#6050 = CARTESIAN_POINT ( 'NONE',  ( -0.1167790944451423535, 4.654944444520310753, 0.2819296736111110424 ) ) ;
#6051 = CARTESIAN_POINT ( 'NONE',  ( 1.337745543335387199E-07, 4.460505239618372642, 0.3119999999999396589 ) ) ;
#6052 = AXIS2_PLACEMENT_3D ( 'NONE', #5923, #17025, #22638 ) ;
#6053 = CARTESIAN_POINT ( 'NONE',  ( -0.1167790944451423535, 4.641055555631422358, 0.2819296736111110424 ) ) ;
#6054 = LINE ( 'NONE', #19104, #16527 ) ;
#6055 = CARTESIAN_POINT ( 'NONE',  ( 0.000000000000000000, 5.384999999999999787, 0.000000000000000000 ) ) ;
#6056 = CARTESIAN_POINT ( 'NONE',  ( -0.3949525857693607089, 5.436648244187127775E-19, 0.06334394204733222178 ) ) ;
#6057 = LINE ( 'NONE', #20939, #8450 ) ;
#6058 = CARTESIAN_POINT ( 'NONE',  ( 0.1292346314604056190, 4.422305555555555934, -0.3119999999999999996 ) ) ;
#6059 = CARTESIAN_POINT ( 'NONE',  ( 0.1993543840281267465, 3.873694444520310309, 0.1993543840281266633 ) ) ;
#6060 =( BOUNDED_CURVE ( )  B_SPLINE_CURVE ( 2, ( #11736, #23045, #6351, #2697, #17573, #8294, #21351, #19276, #863 ),
 .UNSPECIFIED., .F., .F. ) 
 B_SPLINE_CURVE_WITH_KNOTS ( ( 3, 2, 2, 2, 3 ),
 ( 0.1458333333333333703, 0.1562500000000000278, 0.1666666666666666852, 0.1770833333333333703, 0.1875000000000000278 ),
 .UNSPECIFIED. ) 
 CURVE ( )  GEOMETRIC_REPRESENTATION_ITEM ( )  RATIONAL_B_SPLINE_CURVE ( ( 0.9999999999999997780, 0.9238795325112869605, 1.000000000000000000, 0.9238795325112867385, 1.000000000000000000, 0.9238795325112867385, 1.000000000000000000, 0.9238795325112865164, 1.000000000000000222 ) ) 
 REPRESENTATION_ITEM ( '' )  );
#6061 = CARTESIAN_POINT ( 'NONE',  ( -0.3120000000000000551, 0.5423611109593781121, 0.1292346314604056190 ) ) ;
#6062 = APPROVAL_PERSON_ORGANIZATION ( #5257, #19391, #10637 ) ;
#6063 = VERTEX_POINT ( 'NONE', #20505 ) ;
#6064 = DIRECTION ( 'NONE',  ( 0.000000000000000000, 0.000000000000000000, -1.000000000000000000 ) ) ;
#6065 = VERTEX_POINT ( 'NONE', #5383 ) ;
#6066 = CARTESIAN_POINT ( 'NONE',  ( -3.827021247335479543E-17, -0.3125000000000000000, 0.08138888888889088402 ) ) ;
#6067 = CIRCLE ( 'NONE', #5690, 0.6288319206375507786 ) ;
#6068 = CARTESIAN_POINT ( 'NONE',  ( 3.820898013339742174E-17, 5.384999999999999787, 0.3119999999999999996 ) ) ;
#6069 = CARTESIAN_POINT ( 'NONE',  ( -0.3155070326520293400, -0.1306872919485614626, -0.1529861111111109617 ) ) ;
#6070 = CARTESIAN_POINT ( 'NONE',  ( 0.4206476797388901123, 0.2984048262340602276, 0.05816208736408770563 ) ) ;
#6071 = DIRECTION ( 'NONE',  ( 0.7071067811865475727, 1.056266077312805546E-17, -0.7071067811865475727 ) ) ;
#6072 = ORIENTED_EDGE ( 'NONE', *, *, #16045, .F. ) ;
#6073 = CC_DESIGN_SECURITY_CLASSIFICATION ( #2926, ( #4115 ) ) ;
#6074 = CARTESIAN_POINT ( 'NONE',  ( 2.326421213736078119E-17, -0.05982142866897093708, -0.3799334167787516425 ) ) ;
#6075 = CARTESIAN_POINT ( 'NONE',  ( 0.2819296736111110979, 0.4243055554796889006, 0.000000000000000000 ) ) ;
#6076 = CARTESIAN_POINT ( 'NONE',  ( 0.1954553509668046640, -0.1954553509668047195, -0.1061111111111108091 ) ) ;
#6077 = CARTESIAN_POINT ( 'NONE',  ( 0.1398094450097594477, 0.2094524755924680182, -1.227205251919106344 ) ) ;
#6078 = CARTESIAN_POINT ( 'NONE',  ( -0.3060165374364204882, -0.008786209580229879454, -0.09518320410308689361 ) ) ;
#6079 = CARTESIAN_POINT ( 'NONE',  ( -0.1954553509668046640, 0.1954553509668046918, 0.08833333333333517889 ) ) ;
#6080 = CARTESIAN_POINT ( 'NONE',  ( -0.2743877791054161186, 4.617644326071688177, 0.1497255358440195416 ) ) ;
#6081 = DIRECTION ( 'NONE',  ( -0.8660254037844434816, 0.000000000000000000, 0.4999999999999914513 ) ) ;
#6082 = CARTESIAN_POINT ( 'NONE',  ( -0.2048996585731238107, 1.937136306180702348E-16, -0.3358682071059586050 ) ) ;
#6083 = CARTESIAN_POINT ( 'NONE',  ( -0.3119999999999999996, 0.2090277777777773960, -0.1292346314604056745 ) ) ;
#6084 = CARTESIAN_POINT ( 'NONE',  ( -0.2206173157302028232, 5.099388888888888083, -0.2206173157302028232 ) ) ;
#6085 = VECTOR ( 'NONE', #10019, 39.37007874015748143 ) ;
#6086 = CARTESIAN_POINT ( 'NONE',  ( -0.1993543840281266910, 4.193138888964754507, -0.1993543840281266910 ) ) ;
#6087 = CARTESIAN_POINT ( 'NONE',  ( 0.000000000000000000, 3.700000000000000622, 0.000000000000000000 ) ) ;
#6088 = DIRECTION ( 'NONE',  ( 0.5000000000000007772, 0.000000000000000000, 0.8660254037844382635 ) ) ;
#6089 = ORIENTED_EDGE ( 'NONE', *, *, #562, .T. ) ;
#6090 = DIRECTION ( 'NONE',  ( 0.000000000000000000, -0.9961946980917454342, -0.08715574274765833240 ) ) ;
#6091 = CARTESIAN_POINT ( 'NONE',  ( -0.2819296736111110424, 4.738277777853642903, -0.1167790944451423119 ) ) ;
#6092 = CARTESIAN_POINT ( 'NONE',  ( -0.1116596296178200276, 0.4008928570453146878, 0.3436530038418508792 ) ) ;
#6093 = CARTESIAN_POINT ( 'NONE',  ( -0.02658772628240861288, 4.515328577936132959, 0.3108651180470201614 ) ) ;
#6094 = COORDINATED_UNIVERSAL_TIME_OFFSET ( 0, 0, .AHEAD. ) ;
#6095 = CARTESIAN_POINT ( 'NONE',  ( 0.0009813424927043168638, 3.710473627540171293, -0.3119986777745635265 ) ) ;
#6096 = CARTESIAN_POINT ( 'NONE',  ( 0.2206173157302027676, 0.6152777776260449638, 0.2206173157302028787 ) ) ;
#6097 = AXIS2_PLACEMENT_3D ( 'NONE', #14548, #21972, #20150 ) ;
#6098 = CARTESIAN_POINT ( 'NONE',  ( -0.2819296736111110424, 4.314666666742533074, 0.1167790944451424923 ) ) ;
#6099 = COORDINATED_UNIVERSAL_TIME_OFFSET ( 0, 0, .AHEAD. ) ;
#6100 = CARTESIAN_POINT ( 'NONE',  ( -0.2115167397750339906, 4.050456258765779971, -0.2294101962960885810 ) ) ;
#6101 = CARTESIAN_POINT ( 'NONE',  ( -0.1144950937579609779, 0.2764156081756484196, 0.08486111111111295513 ) ) ;
#6102 = CARTESIAN_POINT ( 'NONE',  ( 0.4000000000000000222, 0.2571428571428571175, 0.000000000000000000 ) ) ;
#6103 = CARTESIAN_POINT ( 'NONE',  ( 0.1167790944451423535, 0.4277777777019110550, 0.2819296736111110424 ) ) ;
#6104 = CARTESIAN_POINT ( 'NONE',  ( 3.820898013339742174E-17, 5.384999999999999787, 0.3119999999999999996 ) ) ;
#6105 = CARTESIAN_POINT ( 'NONE',  ( -0.2472135954999579444, 0.3446428569477722470, -0.3402603233408160732 ) ) ;
#6106 = CARTESIAN_POINT ( 'NONE',  ( 0.3236067977499790249, 0.1928571428571428104, -0.2351141009169892826 ) ) ;
#6107 = CARTESIAN_POINT ( 'NONE',  ( -0.3155070326520293400, -0.1306872919485614626, 0.06576388888889039830 ) ) ;
#6108 = CARTESIAN_POINT ( 'NONE',  ( 5.731347020009612645E-17, 3.953555555555555046, 0.3119999999999999996 ) ) ;
#6109 = PLANE ( 'NONE',  #396 ) ;
#6110 = CARTESIAN_POINT ( 'NONE',  ( -0.1167790944451424506, 0.4069444443685778512, 0.2819296736111110424 ) ) ;
#6111 = CARTESIAN_POINT ( 'NONE',  ( -0.1167790944451424368, 0.1291666665908000611, 0.2819296736111110424 ) ) ;
#6112 = ORIENTED_EDGE ( 'NONE', *, *, #18697, .T. ) ;
#6113 = CARTESIAN_POINT ( 'NONE',  ( 0.1993543840281266633, 4.290361111186976828, -0.1993543840281266910 ) ) ;
#6114 = CARTESIAN_POINT ( 'NONE',  ( 0.3236067977499790249, 0.3267857140906294533, -0.2351141009169892826 ) ) ;
#6115 = CARTESIAN_POINT ( 'NONE',  ( -0.2819296736111110424, 4.974388888964754507, -0.1167790944451423119 ) ) ;
#6116 = CARTESIAN_POINT ( 'NONE',  ( -0.1167790944451423535, 4.307722222298088433, 0.2819296736111110979 ) ) ;
#6117 = CARTESIAN_POINT ( 'NONE',  ( 0.4581189881604794123, 0.2644951211353319120, 0.3941886329748525153 ) ) ;
#6118 = VECTOR ( 'NONE', #11441, 39.37007874015748854 ) ;
#6119 = VERTEX_POINT ( 'NONE', #11244 ) ;
#6120 = CARTESIAN_POINT ( 'NONE',  ( 0.3119999999999999996, 4.522999999999999687, -3.820898013339742174E-17 ) ) ;
#6121 = CARTESIAN_POINT ( 'NONE',  ( -0.3119999999999999996, 3.943138889040620931, -0.1292346314604056468 ) ) ;
#6122 = CARTESIAN_POINT ( 'NONE',  ( -7.000945310522701902E-17, 0.4446428569477722803, 0.3999999999999999667 ) ) ;
#6123 = FACE_OUTER_BOUND ( 'NONE', #17004, .T. ) ;
#6124 = VERTEX_POINT ( 'NONE', #20023 ) ;
#6125 = APPROVAL_ROLE ( '' ) ;
#6126 = LINE ( 'NONE', #11885, #10553 ) ;
#6127 = CARTESIAN_POINT ( 'NONE',  ( -0.3104543573706212145, 5.003321778821203658, 0.03789056874165915023 ) ) ;
#6128 = ORIENTED_EDGE ( 'NONE', *, *, #11014, .T. ) ;
#6129 = CARTESIAN_POINT ( 'NONE',  ( 0.1993543840281266355, 0.1534722221463556135, 0.1993543840281267465 ) ) ;
#6130 = VECTOR ( 'NONE', #16083, 39.37007874015748143 ) ;
#6131 = ORIENTED_EDGE ( 'NONE', *, *, #14723, .F. ) ;
#6132 = CARTESIAN_POINT ( 'NONE',  ( 0.03688365757930828215, 4.265052467647925560, -0.3099171647324295287 ) ) ;
#6133 = CARTESIAN_POINT ( 'NONE',  ( 0.1943163256447900666, 0.4290772944463143168, 0.4279515871991319553 ) ) ;
#6134 = CARTESIAN_POINT ( 'NONE',  ( 0.3121991201319634923, 4.753296228494991560, -0.04110499377590303566 ) ) ;
#6135 = CARTESIAN_POINT ( 'NONE',  ( -0.2233192592356399997, 0.1116071427596004306, 0.3073725909049499494 ) ) ;
#6136 = CARTESIAN_POINT ( 'NONE',  ( 0.2838754445270939009, 5.176981630833639159, 0.07949240647762143008 ) ) ;
#6137 = ORIENTED_EDGE ( 'NONE', *, *, #17286, .F. ) ;
#6138 = ADVANCED_FACE ( 'NONE', ( #134 ), #9651, .T. ) ;
#6139 = CARTESIAN_POINT ( 'NONE',  ( -0.2233192592356399442, 0.2508928570453147211, -0.3073725909049499494 ) ) ;
#6140 = CARTESIAN_POINT ( 'NONE',  ( -1.910449006669871087E-17, 3.870222222222221564, -0.3119999999999999996 ) ) ;
#6141 = CARTESIAN_POINT ( 'NONE',  ( -0.1144950937579609918, -0.2764156081756484196, 0.4320833333333379822 ) ) ;
#6142 = CARTESIAN_POINT ( 'NONE',  ( -0.1167790944451423257, 3.898000000075865668, -0.2819296736111110424 ) ) ;
#6143 = CARTESIAN_POINT ( 'NONE',  ( 0.000000000000000000, 5.580000000000000959, 0.000000000000000000 ) ) ;
#6144 = CARTESIAN_POINT ( 'NONE',  ( -0.2786158314465964625, 5.183151893613593408, 0.08921164663449078491 ) ) ;
#6145 = CARTESIAN_POINT ( 'NONE',  ( -0.3119999999999998885, 4.450083333485065573, 0.1292346314604058410 ) ) ;
#6146 = EDGE_CURVE ( 'NONE', #10162, #22655, #6223, .T. ) ;
#6147 = CARTESIAN_POINT ( 'NONE',  ( 5.178964085587577574E-17, 4.880638888964754507, 0.2819296736111110979 ) ) ;
#6148 = ORIENTED_EDGE ( 'NONE', *, *, #8461, .F. ) ;
#6149 = CARTESIAN_POINT ( 'NONE',  ( 0.2819296736111110979, 4.269527777853643791, -3.452642723725051716E-17 ) ) ;
#6150 = AXIS2_PLACEMENT_3D ( 'NONE', #7135, #16405, #20414 ) ;
#6151 = ORIENTED_EDGE ( 'NONE', *, *, #179, .F. ) ;
#6152 = CARTESIAN_POINT ( 'NONE',  ( -0.1116596296178199582, 0.3008928570453147100, -0.3436530038418508792 ) ) ;
#6153 = ORIENTED_EDGE ( 'NONE', *, *, #1453, .T. ) ;
#6154 = VERTEX_POINT ( 'NONE', #8168 ) ;
#6155 = DATE_AND_TIME ( #9953, #15383 ) ;
#6156 = ORIENTED_EDGE ( 'NONE', *, *, #20625, .F. ) ;
#6157 = CARTESIAN_POINT ( 'NONE',  ( 0.000000000000000000, 0.3155070326520292845, 0.3852083333333378157 ) ) ;
#6158 = CARTESIAN_POINT ( 'NONE',  ( 0.1292346314604056745, 0.3062499999999995781, -0.3119999999999999996 ) ) ;
#6159 = CARTESIAN_POINT ( 'NONE',  ( -1.726321361862525858E-17, 3.741750000075865668, -0.2819296736111110979 ) ) ;
#6160 = CARTESIAN_POINT ( 'NONE',  ( 0.2614991890488166937, 4.413735171690442272, 0.1718472760850429104 ) ) ;
#6161 = CARTESIAN_POINT ( 'NONE',  ( -0.1294417382415922746, -0.3125000000000000000, -0.08874999999999934330 ) ) ;
#6162 = EDGE_CURVE ( 'NONE', #4761, #17737, #7744, .T. ) ;
#6163 = CARTESIAN_POINT ( 'NONE',  ( -0.3119999999999999996, 4.939666666666665762, 0.000000000000000000 ) ) ;
#6164 = EDGE_CURVE ( 'NONE', #20369, #11906, #4034, .T. ) ;
#6165 = VECTOR ( 'NONE', #6287, 39.37007874015748854 ) ;
#6166 = CARTESIAN_POINT ( 'NONE',  ( 0.2764156081756483641, 0.1144950937579610195, 0.2306944444444475328 ) ) ;
#6167 = CARTESIAN_POINT ( 'NONE',  ( -0.1167790944451424506, 0.4763888888130222155, 0.2819296736111110424 ) ) ;
#6168 = CARTESIAN_POINT ( 'NONE',  ( -0.1954553509668046640, 0.1954553509668046918, 0.3661111111111151617 ) ) ;
#6169 = ORIENTED_EDGE ( 'NONE', *, *, #17076, .F. ) ;
#6170 = CARTESIAN_POINT ( 'NONE',  ( 0.1993543840281267465, 4.720916666742533074, 0.1993543840281266633 ) ) ;
#6171 = CARTESIAN_POINT ( 'NONE',  ( -0.3999999999999999667, 0.4232142855192009279, -0.1299678784931626030 ) ) ;
#6172 = CARTESIAN_POINT ( 'NONE',  ( -0.1993543840281266355, 4.637583333409198261, 0.1993543840281267465 ) ) ;
#6173 = CARTESIAN_POINT ( 'NONE',  ( 0.2206173157302027676, 0.2819444442927114824, 0.2206173157302028787 ) ) ;
#6174 = CARTESIAN_POINT ( 'NONE',  ( -0.2209708691207961373, -0.2209708691207961095, 0.3452777777777815138 ) ) ;
#6175 = CARTESIAN_POINT ( 'NONE',  ( -0.06281267474701307529, 1.673690498276176774E-18, 0.3705465256992553913 ) ) ;
#6176 = FACE_OUTER_BOUND ( 'NONE', #5082, .T. ) ;
#6177 = CARTESIAN_POINT ( 'NONE',  ( -0.1292346314604056745, 4.207027777777777366, -0.3119999999999999996 ) ) ;
#6178 = B_SPLINE_CURVE_WITH_KNOTS ( 'NONE', 3,
 ( #5460, #18148, #23854, #5086, #21915, #10713, #14746, #1680 ),
 .UNSPECIFIED., .F., .F.,
 ( 4, 2, 2, 4 ),
 ( 0.000000000000000000, 0.0004997454757086407804, 0.0007496182135629599237, 0.0009994909514172789586 ),
 .UNSPECIFIED. ) ;
#6179 = CARTESIAN_POINT ( 'NONE',  ( -1.726321361862525858E-17, 3.727861111186976384, -0.2819296736111110979 ) ) ;
#6180 = EDGE_CURVE ( 'NONE', #13004, #22501, #17390, .T. ) ;
#6181 = CARTESIAN_POINT ( 'NONE',  ( 2.986000000000000210, 2.690000000000002167, -2.541000000000000369 ) ) ;
#6182 = ORIENTED_EDGE ( 'NONE', *, *, #23687, .T. ) ;
#6183 = CARTESIAN_POINT ( 'NONE',  ( 0.3247595264191652786, 2.685901063997345961, -1.021671737322407791 ) ) ;
#6184 = ORIENTED_EDGE ( 'NONE', *, *, #14253, .T. ) ;
#6185 = CARTESIAN_POINT ( 'NONE',  ( 0.2792411303351374219, 4.700719259618558965, -0.1393336886063105129 ) ) ;
#6186 = AXIS2_PLACEMENT_3D ( 'NONE', #10064, #9369, #18878 ) ;
#6187 = CARTESIAN_POINT ( 'NONE',  ( 0.1907726824043486646, 4.133016981313245353, 0.2468801249805909759 ) ) ;
#6188 = CARTESIAN_POINT ( 'NONE',  ( -0.2230971623002954152, -0.2230971623002953874, -0.09395833333333269977 ) ) ;
#6189 = CARTESIAN_POINT ( 'NONE',  ( -0.0003188451214018954817, 3.932731264085634670, -0.3119998472765105890 ) ) ;
#6190 = VERTEX_POINT ( 'NONE', #7760 ) ;
#6191 = ADVANCED_FACE ( 'NONE', ( #16698 ), #14635, .T. ) ;
#6192 = CARTESIAN_POINT ( 'NONE',  ( 0.1116596296178199027, 0.4258928570453147100, 0.3436530038418508792 ) ) ;
#6193 = CARTESIAN_POINT ( 'NONE',  ( 0.1993543840281266910, 0.5423611110352445364, -0.1993543840281266910 ) ) ;
#6194 = CARTESIAN_POINT ( 'NONE',  ( -0.1954553509668046640, 0.1954553509668046918, -0.1338888888888887796 ) ) ;
#6195 = CARTESIAN_POINT ( 'NONE',  ( 0.2675580960581577239, 0.3158763822996886739, -1.176569835631964045 ) ) ;
#6196 = CARTESIAN_POINT ( 'NONE',  ( -5.731347020009612645E-17, 0.5041666666666663188, 0.3119999999999999996 ) ) ;
#6197 = CARTESIAN_POINT ( 'NONE',  ( 0.2764156081756483641, 0.1144950937579610056, 0.1820833333333359283 ) ) ;
#6198 = ORIENTED_EDGE ( 'NONE', *, *, #2331, .F. ) ;
#6199 =( BOUNDED_CURVE ( )  B_SPLINE_CURVE ( 2, ( #1608, #18666, #9160, #1838, #1486, #18427, #3672, #1966, #9042, #5378, #16488, #7573, #3549 ),
 .UNSPECIFIED., .F., .F. ) 
 B_SPLINE_CURVE_WITH_KNOTS ( ( 3, 2, 2, 2, 2, 2, 3 ),
 ( 0.5357142857142856984, 0.5428571428571428159, 0.5571428571428571619, 0.5714285714285713969, 0.5857142857142857428, 0.5999999999999999778, 0.6071428571428572063 ),
 .UNSPECIFIED. ) 
 CURVE ( )  GEOMETRIC_REPRESENTATION_ITEM ( )  RATIONAL_B_SPLINE_CURVE ( ( 0.9755282581475768211, 0.9755282581475768211, 1.000000000000000000, 0.9510565162951535312, 1.000000000000000000, 0.9510565162951535312, 1.000000000000000000, 0.9510565162951535312, 1.000000000000000000, 0.9510565162951535312, 1.000000000000000000, 0.9755282581475765991, 0.9755282581475768211 ) ) 
 REPRESENTATION_ITEM ( '' )  );
#6200 = CARTESIAN_POINT ( 'NONE',  ( -0.2048285092061691848, 5.112368305460988971, 0.2322580485435521980 ) ) ;
#6201 = LINE ( 'NONE', #11829, #21812 ) ;
#6202 = CARTESIAN_POINT ( 'NONE',  ( 0.1952751578279883771, -4.088425335522479322E-18, -0.3153013832115701409 ) ) ;
#6203 = CARTESIAN_POINT ( 'NONE',  ( 1.910449006669871087E-17, 0.1430555555555552139, -0.3119999999999999996 ) ) ;
#6204 = CARTESIAN_POINT ( 'NONE',  ( 0.3119999999999999996, 4.852861111111110404, 0.1292346314604056190 ) ) ;
#6205 = AXIS2_PLACEMENT_3D ( 'NONE', #2948, #10282, #10406 ) ;
#6206 = CARTESIAN_POINT ( 'NONE',  ( 0.2819296736111110979, 3.894527777853643347, -3.452642723725051716E-17 ) ) ;
#6207 = EDGE_CURVE ( 'NONE', #22719, #16849, #1582, .T. ) ;
#6208 = CARTESIAN_POINT ( 'NONE',  ( -0.2726800006319771708, 4.330919655780821387, -0.1570310010236034837 ) ) ;
#6209 = CARTESIAN_POINT ( 'NONE',  ( -1.889944503261478141E-16, 0.5289902422706634910, 0.3941886329748526263 ) ) ;
#6210 = DIRECTION ( 'NONE',  ( -0.000000000000000000, -1.000000000000000000, -0.000000000000000000 ) ) ;
#6211 = VERTEX_POINT ( 'NONE', #3645 ) ;
#6212 = CARTESIAN_POINT ( 'NONE',  ( -0.4788451055546355528, -0.2690082051306183497, 0.04193467568257207984 ) ) ;
#6213 = CARTESIAN_POINT ( 'NONE',  ( -1.726321361862525858E-17, 4.727861111186976828, -0.2819296736111110979 ) ) ;
#6214 = CARTESIAN_POINT ( 'NONE',  ( 0.4254287158503464727, -0.3089275304546717504, 0.05347130368200839895 ) ) ;
#6215 = DIRECTION ( 'NONE',  ( -0.000000000000000000, -1.000000000000000000, -0.000000000000000000 ) ) ;
#6216 = CALENDAR_DATE ( 2026, 7, 10 ) ;
#6217 = CARTESIAN_POINT ( 'NONE',  ( 0.000000000000000000, 0.01999999999999951469, 0.000000000000000000 ) ) ;
#6218 = DIRECTION ( 'NONE',  ( 1.000000000000000000, 0.000000000000000000, -6.148297094540788948E-16 ) ) ;
#6219 = ADVANCED_BREP_SHAPE_REPRESENTATION ( '', ( #9145, #9127 ), #558 ) ;
#6220 = VECTOR ( 'NONE', #17576, 39.37007874015748143 ) ;
#6221 = CARTESIAN_POINT ( 'NONE',  ( -0.1993543840281266355, 4.373694444520309865, 0.1993543840281267465 ) ) ;
#6222 = CARTESIAN_POINT ( 'NONE',  ( -0.4593750000000003664, -6.734002413227273428E-17, 0.4343810118395207698 ) ) ;
#6223 = LINE ( 'NONE', #13571, #18252 ) ;
#6224 = CARTESIAN_POINT ( 'NONE',  ( 0.4500000000000003442, 0.2598076211353319009, 0.3779506566538943235 ) ) ;
#6225 = CARTESIAN_POINT ( 'NONE',  ( -0.1993543840281266633, 0.4590277777019112215, -0.1993543840281266910 ) ) ;
#6226 = LINE ( 'NONE', #7701, #2994 ) ;
#6227 = CARTESIAN_POINT ( 'NONE',  ( 0.000000000000000000, 3.575000000000000622, 0.000000000000000000 ) ) ;
#6228 = CARTESIAN_POINT ( 'NONE',  ( 3.820898013339742174E-17, 5.384999999999999787, 0.3119999999999999996 ) ) ;
#6229 = CARTESIAN_POINT ( 'NONE',  ( -0.3155070326520293400, -0.1306872919485614626, 0.1213194444444463810 ) ) ;
#6230 = DIRECTION ( 'NONE',  ( 0.000000000000000000, -1.000000000000000000, 0.000000000000000000 ) ) ;
#6231 = CARTESIAN_POINT ( 'NONE',  ( 1.519200945994765378E-06, 3.766055514889470324, -0.3119999999963013471 ) ) ;
#6232 = CARTESIAN_POINT ( 'NONE',  ( 0.2819296736111110424, 0.4208333332574666907, 0.1167790944451424923 ) ) ;
#6233 = CARTESIAN_POINT ( 'NONE',  ( -5.178964085587577574E-17, 0.1326388888130222710, 0.2819296736111110979 ) ) ;
#6234 = CARTESIAN_POINT ( 'NONE',  ( -0.2819296736111110424, 4.092444444520309865, 0.1167790944451424923 ) ) ;
#6235 = CARTESIAN_POINT ( 'NONE',  ( -7.726019084026502927E-17, 0.3732142855192007724, 0.4205848896953069405 ) ) ;
#6236 = EDGE_CURVE ( 'NONE', #18304, #2863, #5957, .T. ) ;
#6237 = CARTESIAN_POINT ( 'NONE',  ( -1.726321361862525858E-17, 4.963972222298088433, -0.2819296736111110979 ) ) ;
#6238 = AXIS2_PLACEMENT_3D ( 'NONE', #17538, #21789, #4839 ) ;
#6239 = LINE ( 'NONE', #1990, #8279 ) ;
#6240 = VECTOR ( 'NONE', #19156, 39.37007874015748143 ) ;
#6241 = ORIENTED_EDGE ( 'NONE', *, *, #4244, .F. ) ;
#6242 = CARTESIAN_POINT ( 'NONE',  ( -0.5116234456863258950, 1.999640111863030478, -2.640781157734871876 ) ) ;
#6243 = CARTESIAN_POINT ( 'NONE',  ( 0.3119999999999999996, 3.804250000151731648, 0.1292346314604056190 ) ) ;
#6244 = DIRECTION ( 'NONE',  ( 0.000000000000000000, 0.000000000000000000, -1.000000000000000000 ) ) ;
#6245 =( BOUNDED_CURVE ( )  B_SPLINE_CURVE ( 2, ( #8013, #21187, #9984, #4600, #6066, #10221, #13405, #12059, #2655 ),
 .UNSPECIFIED., .F., .T. ) 
 B_SPLINE_CURVE_WITH_KNOTS ( ( 3, 2, 2, 2, 3 ),
 ( 0.5312500000000001110, 0.5416666666666668517, 0.5520833333333334814, 0.5625000000000000000, 0.5729166666666667407 ),
 .UNSPECIFIED. ) 
 CURVE ( )  GEOMETRIC_REPRESENTATION_ITEM ( )  RATIONAL_B_SPLINE_CURVE ( ( 0.9999999999999992228, 0.9238795325112875156, 1.000000000000000000, 0.9238795325112867385, 1.000000000000000000, 0.9238795325112867385, 1.000000000000000000, 0.9238795325112867385, 1.000000000000000000 ) ) 
 REPRESENTATION_ITEM ( '' )  );
#6246 =( CONVERSION_BASED_UNIT ( 'INCH', #761 ) LENGTH_UNIT ( ) NAMED_UNIT ( #4788 ) );
#6247 = ORIENTED_EDGE ( 'NONE', *, *, #15293, .F. ) ;
#6248 = APPROVAL_DATE_TIME ( #19537, #21485 ) ;
#6249 = ORIENTED_EDGE ( 'NONE', *, *, #16291, .F. ) ;
#6250 = CARTESIAN_POINT ( 'NONE',  ( 0.3999999999999999667, 0.3321428571428570176, -0.1299678784931625197 ) ) ;
#6251 = CIRCLE ( 'NONE', #9376, 0.6211549996190571798 ) ;
#6252 = CARTESIAN_POINT ( 'NONE',  ( -0.1908996484622546286, 5.010266985262351369, 0.2504379711342784032 ) ) ;
#6253 = VERTEX_POINT ( 'NONE', #9257 ) ;
#6254 = CARTESIAN_POINT ( 'NONE',  ( 0.1993543840281266910, 0.1118055554796889145, -0.1993543840281266910 ) ) ;
#6255 = VECTOR ( 'NONE', #7018, 39.37007874015748143 ) ;
#6256 = CARTESIAN_POINT ( 'NONE',  ( 0.2860402380377710108, 4.255804247949799723, -0.1246337105255282962 ) ) ;
#6257 = CARTESIAN_POINT ( 'NONE',  ( 0.3832388449590170554, 0.3084783300535419159, 0.4166279060364238562 ) ) ;
#6258 = CARTESIAN_POINT ( 'NONE',  ( 0.1161582368758659611, 4.075052052462464047, 0.2903959765898691536 ) ) ;
#6259 = CARTESIAN_POINT ( 'NONE',  ( -0.3613381517857143232, 0.1687499999024575370, -0.1174058825155741004 ) ) ;
#6260 = DIRECTION ( 'NONE',  ( -0.7071067811865474617, 0.000000000000000000, 0.7071067811865474617 ) ) ;
#6261 = CC_DESIGN_PERSON_AND_ORGANIZATION_ASSIGNMENT ( #17021, #4088, ( #12267 ) ) ;
#6262 = ORIENTED_EDGE ( 'NONE', *, *, #19344, .F. ) ;
#6263 = CARTESIAN_POINT ( 'NONE',  ( -0.2233192592356400275, 0.2723214284738861291, 0.3073725909049499494 ) ) ;
#6264 = CARTESIAN_POINT ( 'NONE',  ( -0.1236067977499789583, 0.1267857140906294700, -0.3804226065180614791 ) ) ;
#6265 = B_SPLINE_CURVE_WITH_KNOTS ( 'NONE', 3,
 ( #15528, #4422, #11638, #7959, #6252, #13595, #7842, #17239, #10050, #11887, #648, #17356, #766, #21008, #6008, #19180, #19302, #522, #4184, #9681, #2489, #6127, #4301, #13823, #15289, #15647, #23067, #22606, #6375, #21257, #4545, #12008, #22718, #2117, #19063, #7725, #284, #15171, #20772, #4061 ),
 .UNSPECIFIED., .F., .F.,
 ( 4, 2, 2, 1, 2, 2, 1, 1, 2, 2, 2, 2, 2, 2, 2, 2, 1, 2, 2, 2, 2, 4 ),
 ( 0.1370976352218340188, 0.1393776508289605309, 0.1416576664360870708, 0.1418001674115324795, 0.1418714178992551700, 0.1418892305211858496, 0.1419070431431165291, 0.1419426683869778882, 0.1422276703378687057, 0.1427976742396503407, 0.1439376820432136383, 0.1450776898467769360, 0.1462176976503402059, 0.1473577054539035036, 0.1479277093556851386, 0.1482127113065759560, 0.1483552122820213925, 0.1484264627697440830, 0.1484977132574668013, 0.1507777288645933411, 0.1530577444717199087, 0.1553377600788464485 ),
 .UNSPECIFIED. ) ;
#6266 = CARTESIAN_POINT ( 'NONE',  ( -0.2819296736111110424, 3.960500000075865668, -0.1167790944451423119 ) ) ;
#6267 = CARTESIAN_POINT ( 'NONE',  ( -0.4208772603875798324, -0.2863811090246152768, 0.4064915563616229299 ) ) ;
#6268 = CARTESIAN_POINT ( 'NONE',  ( -0.09411960903131520728, 5.165948514229523170, -0.2827352314489141594 ) ) ;
#6269 = CARTESIAN_POINT ( 'NONE',  ( 0.3119999999999999996, 4.415361111262844140, 0.1292346314604056190 ) ) ;
#6270 = CARTESIAN_POINT ( 'NONE',  ( 0.1993543840281266633, 4.845916666742532186, -0.1993543840281266910 ) ) ;
#6271 = VERTEX_POINT ( 'NONE', #1697 ) ;
#6272 = VECTOR ( 'NONE', #5023, 39.37007874015748143 ) ;
#6273 = CARTESIAN_POINT ( 'NONE',  ( 0.1167790944451424368, 3.981333333409199593, 0.2819296736111110424 ) ) ;
#6274 = VERTEX_POINT ( 'NONE', #9134 ) ;
#6275 = CARTESIAN_POINT ( 'NONE',  ( -0.3613381517857143232, 0.2437499999024575481, -4.425116109941954795E-17 ) ) ;
#6276 = VERTEX_POINT ( 'NONE', #5478 ) ;
#6277 = EDGE_CURVE ( 'NONE', #21887, #10641, #14390, .T. ) ;
#6278 = VERTEX_POINT ( 'NONE', #16339 ) ;
#6279 = APPROVAL_DATE_TIME ( #20918, #5204 ) ;
#6280 = ORIENTED_EDGE ( 'NONE', *, *, #23306, .F. ) ;
#6281 = CYLINDRICAL_SURFACE ( 'NONE', #17706, 0.4062499999999997780 ) ;
#6282 = CARTESIAN_POINT ( 'NONE',  ( -0.1294417382415922191, 0.3125000000000000000, 0.2723611111111142735 ) ) ;
#6283 = CARTESIAN_POINT ( 'NONE',  ( -0.3119999999999999996, 0.04236111095937818150, 0.1292346314604056190 ) ) ;
#6284 = CARTESIAN_POINT ( 'NONE',  ( 0.2724733894366830889, 5.141277903277533312, 0.1372292302282890064 ) ) ;
#6285 = PRODUCT_RELATED_PRODUCT_CATEGORY ( 'detail', '', ( #7006 ) ) ;
#6286 = CARTESIAN_POINT ( 'NONE',  ( -0.4687500000000004996, 0.08992298774708656905, 0.4251082876142271982 ) ) ;
#6287 = DIRECTION ( 'NONE',  ( 0.8090181274631199626, 0.5597738724868831506, 0.1792843582611305941 ) ) ;
#6288 = CARTESIAN_POINT ( 'NONE',  ( -0.5116234456863466562, 3.514980167629567998, 2.949589416182695878 ) ) ;
#6289 = ORIENTED_EDGE ( 'NONE', *, *, #16454, .T. ) ;
#6290 = CARTESIAN_POINT ( 'NONE',  ( -0.1144950937579609918, -0.2764156081756484196, 0.3209722222222259891 ) ) ;
#6291 = CARTESIAN_POINT ( 'NONE',  ( -0.1993543840281266633, 0.1118055554796889145, -0.1993543840281266910 ) ) ;
#6292 = CARTESIAN_POINT ( 'NONE',  ( 0.000000000000000000, 0.2764156081756484196, 0.3591666666666706309 ) ) ;
#6293 = ORIENTED_EDGE ( 'NONE', *, *, #20654, .F. ) ;
#6294 = CARTESIAN_POINT ( 'NONE',  ( -0.1993543840281266355, 4.762583333409199149, 0.1993543840281267465 ) ) ;
#6295 = CARTESIAN_POINT ( 'NONE',  ( 0.4581189881604794123, -0.2644951211353317455, 0.3941886329748525153 ) ) ;
#6296 = CARTESIAN_POINT ( 'NONE',  ( 0.1993543840281266633, 4.720916666742532186, -0.1993543840281266910 ) ) ;
#6297 = CARTESIAN_POINT ( 'NONE',  ( 0.4588877537281843555, -0.1552297620431791481, 0.4201833234654208660 ) ) ;
#6298 = CARTESIAN_POINT ( 'NONE',  ( 0.2347259105283345526, 4.856899042655335563, 0.2057643236453879643 ) ) ;
#6299 = CARTESIAN_POINT ( 'NONE',  ( 0.000000000000000000, 0.000000000000000000, 1.326383476483184332 ) ) ;
#6300 = CARTESIAN_POINT ( 'NONE',  ( -0.4620775622572422248, 0.2744852724095708241, 0.05975564523638852987 ) ) ;
#6301 = CARTESIAN_POINT ( 'NONE',  ( -0.3119999999999998885, 4.332027777777778255, 0.1292346314604058410 ) ) ;
#6302 = CARTESIAN_POINT ( 'NONE',  ( 5.731347020009612645E-17, 5.182722222373954857, 0.3119999999999999996 ) ) ;
#6303 = CARTESIAN_POINT ( 'NONE',  ( -0.3116633505738114485, 3.673292957400295933, 0.09499999999999995948 ) ) ;
#6304 = ORIENTED_EDGE ( 'NONE', *, *, #20311, .F. ) ;
#6305 = CARTESIAN_POINT ( 'NONE',  ( 0.1963876315374232240, 0.4278814254316301580, 0.09139303015897916327 ) ) ;
#6306 = ORIENTED_EDGE ( 'NONE', *, *, #20136, .F. ) ;
#6307 = CARTESIAN_POINT ( 'NONE',  ( 0.0007589115252507630483, 4.710479605489643617, -0.3119992096284730509 ) ) ;
#6308 = EDGE_CURVE ( 'NONE', #19422, #14487, #10086, .T. ) ;
#6309 = DESIGN_CONTEXT ( 'detailed design', #23042, 'design' ) ;
#6310 = CARTESIAN_POINT ( 'NONE',  ( 0.1049994648621434823, 4.130212265090358770, 0.2947840903239055677 ) ) ;
#6311 = CARTESIAN_POINT ( 'NONE',  ( -0.3155070326520292845, 1.931923388228935888E-17, 0.1213194444444467696 ) ) ;
#6312 = CARTESIAN_POINT ( 'NONE',  ( 0.2727449834095620473, 4.312289586052585832, -0.1569221876317137276 ) ) ;
#6313 = ADVANCED_FACE ( 'NONE', ( #16221 ), #1461, .T. ) ;
#6314 = CARTESIAN_POINT ( 'NONE',  ( 0.2923287055106771337, 0.05803571418817188299, 0.2123892367102621359 ) ) ;
#6315 = CARTESIAN_POINT ( 'NONE',  ( 0.1167790944451423535, 0.4694444443685777957, 0.2819296736111110424 ) ) ;
#6316 = DIRECTION ( 'NONE',  ( -0.000000000000000000, -1.000000000000000000, -0.000000000000000000 ) ) ;
#6317 = DIRECTION ( 'NONE',  ( -0.000000000000000000, -0.000000000000000000, -1.000000000000000000 ) ) ;
#6318 = CARTESIAN_POINT ( 'NONE',  ( -0.009375000000000190473, 0.5358532185916217161, 0.06112444011295373181 ) ) ;
#6319 = CARTESIAN_POINT ( 'NONE',  ( 0.1144950937579609085, -0.2764156081756484751, 0.2237500000000028910 ) ) ;
#6320 = VERTEX_POINT ( 'NONE', #3281 ) ;
#6321 = DIRECTION ( 'NONE',  ( -0.000000000000000000, -1.000000000000000000, -0.000000000000000000 ) ) ;
#6322 = CARTESIAN_POINT ( 'NONE',  ( -0.006528205157002933690, 0.5487477722931475288, 0.04212966708837333901 ) ) ;
#6323 = DIRECTION ( 'NONE',  ( 0.000000000000000000, 1.000000000000000000, 0.000000000000000000 ) ) ;
#6324 = CARTESIAN_POINT ( 'NONE',  ( -0.3119999999999999996, 0.3791666666666663188, -3.820898013339742174E-17 ) ) ;
#6325 = CARTESIAN_POINT ( 'NONE',  ( -0.2206173157302028232, 4.877166666666665762, -0.2206173157302028232 ) ) ;
#6326 = CARTESIAN_POINT ( 'NONE',  ( 0.1993543840281267465, 3.998694444520310753, 0.1993543840281266633 ) ) ;
#6327 = DIRECTION ( 'NONE',  ( -0.000000000000000000, 0.000000000000000000, -1.000000000000000000 ) ) ;
#6328 = CARTESIAN_POINT ( 'NONE',  ( -0.03741580292205138464, 0.5077710590217058284, 0.4064395341356222269 ) ) ;
#6329 = CARTESIAN_POINT ( 'NONE',  ( 0.3065849364905491314, 4.945545817829770315E-15, 0.4182516031572158233 ) ) ;
#6330 = ORIENTED_EDGE ( 'NONE', *, *, #23214, .T. ) ;
#6331 = LINE ( 'NONE', #13786, #4657 ) ;
#6332 = CARTESIAN_POINT ( 'NONE',  ( 0.2819296736111110979, 4.825083333409199149, -3.452642723725051716E-17 ) ) ;
#6333 = AXIS2_PLACEMENT_3D ( 'NONE', #13896, #21325, #17546 ) ;
#6334 = CARTESIAN_POINT ( 'NONE',  ( 0.08339729271156200163, 0.4931164279685679719, 0.07808165802387295740 ) ) ;
#6335 = EDGE_CURVE ( 'NONE', #8700, #9142, #11344, .T. ) ;
#6336 = CARTESIAN_POINT ( 'NONE',  ( 0.08311813270112124175, -0.4932776010757431440, 0.4002893343786021463 ) ) ;
#6337 = EDGE_CURVE ( 'NONE', #8276, #18019, #21044, .T. ) ;
#6338 = APPROVAL_DATE_TIME ( #23034, #23394 ) ;
#6339 = CARTESIAN_POINT ( 'NONE',  ( -1.403438536077215402E-16, 0.9040586665785882436, -1.048989065017511546 ) ) ;
#6340 = DIRECTION ( 'NONE',  ( 0.000000000000000000, 1.000000000000000000, 0.000000000000000000 ) ) ;
#6341 = CARTESIAN_POINT ( 'NONE',  ( -1.726321361862525858E-17, 4.241750000075866112, -0.2819296736111110979 ) ) ;
#6342 = EDGE_CURVE ( 'NONE', #22119, #10448, #20669, .T. ) ;
#6343 = CARTESIAN_POINT ( 'NONE',  ( -0.01686310874185860051, 4.044291452137212417, -0.3115464117857045800 ) ) ;
#6344 =( BOUNDED_CURVE ( )  B_SPLINE_CURVE ( 2, ( #19106, #2411, #6174, #19221, #9973, #17400, #22994, #21176, #5815 ),
 .UNSPECIFIED., .F., .F. ) 
 B_SPLINE_CURVE_WITH_KNOTS ( ( 3, 2, 2, 2, 3 ),
 ( 0.6875000000000001110, 0.6979166666666667407, 0.7083333333333334814, 0.7187500000000000000, 0.7291666666666666297 ),
 .UNSPECIFIED. ) 
 CURVE ( )  GEOMETRIC_REPRESENTATION_ITEM ( )  RATIONAL_B_SPLINE_CURVE ( ( 0.9999999999999992228, 0.9238795325112875156, 1.000000000000000000, 0.9238795325112867385, 1.000000000000000000, 0.9238795325112867385, 1.000000000000000000, 0.9238795325112867385, 1.000000000000000000 ) ) 
 REPRESENTATION_ITEM ( '' )  );
#6345 = CARTESIAN_POINT ( 'NONE',  ( -0.1144950937579609779, 0.2764156081756484196, 0.2515277777777809587 ) ) ;
#6346 =( BOUNDED_CURVE ( )  B_SPLINE_CURVE ( 2, ( #7567, #9640, #11474, #22678, #5968, #19030, #9763, #5852, #11598 ),
 .UNSPECIFIED., .F., .F. ) 
 B_SPLINE_CURVE_WITH_KNOTS ( ( 3, 2, 2, 2, 3 ),
 ( 0.5625000000000000000, 0.5729166666666666297, 0.5833333333333333703, 0.5937500000000000000, 0.6041666666666666297 ),
 .UNSPECIFIED. ) 
 CURVE ( )  GEOMETRIC_REPRESENTATION_ITEM ( )  RATIONAL_B_SPLINE_CURVE ( ( 1.000000000000000000, 0.9238795325112867385, 1.000000000000000000, 0.9238795325112867385, 1.000000000000000000, 0.9238795325112867385, 1.000000000000000000, 0.9238795325112867385, 1.000000000000000000 ) ) 
 REPRESENTATION_ITEM ( '' )  );
#6347 = CARTESIAN_POINT ( 'NONE',  ( 0.3255746755405797832, 3.686631053106446565, 0.09499999999999995948 ) ) ;
#6348 = CARTESIAN_POINT ( 'NONE',  ( -0.1167790944451422702, 0.3999999999241334869, -0.2819296736111110424 ) ) ;
#6349 = CARTESIAN_POINT ( 'NONE',  ( -0.3119999999999999996, 0.4312499999999996891, -0.1292346314604056745 ) ) ;
#6350 = CARTESIAN_POINT ( 'NONE',  ( 0.3119999999999999996, 4.470916666666665762, -0.1292346314604056745 ) ) ;
#6351 = CARTESIAN_POINT ( 'NONE',  ( 0.2209708691207961651, 0.2209708691207959985, -0.01583333333333248119 ) ) ;
#6352 = CARTESIAN_POINT ( 'NONE',  ( 0.3155070326520292290, -0.1306872919485616569, 0.1421527777777798485 ) ) ;
#6353 = AXIS2_PLACEMENT_3D ( 'NONE', #15638, #13934, #6602 ) ;
#6354 = VERTEX_POINT ( 'NONE', #7993 ) ;
#6355 = DIRECTION ( 'NONE',  ( 0.000000000000000000, 0.000000000000000000, -1.000000000000000000 ) ) ;
#6356 = CARTESIAN_POINT ( 'NONE',  ( -0.008920037193760966057, 3.766295647218201648, -0.3118907412506480847 ) ) ;
#6357 = CARTESIAN_POINT ( 'NONE',  ( 0.2819296736111110979, 0.4798611110352444808, 0.000000000000000000 ) ) ;
#6358 = CARTESIAN_POINT ( 'NONE',  ( -0.1167790944451424368, 0.2402777777019111660, 0.2819296736111110424 ) ) ;
#6359 = CARTESIAN_POINT ( 'NONE',  ( 0.1167790944451424368, 4.106333333409199149, 0.2819296736111110424 ) ) ;
#6360 = CARTESIAN_POINT ( 'NONE',  ( -0.2472135954999579999, 0.3660714283763437660, 0.3402603233408159622 ) ) ;
#6361 = EDGE_CURVE ( 'NONE', #12233, #16427, #6527, .T. ) ;
#6362 = CARTESIAN_POINT ( 'NONE',  ( -1.726321361862525858E-17, 4.630638888964754507, -0.2819296736111110979 ) ) ;
#6363 = CARTESIAN_POINT ( 'NONE',  ( 0.3119999999999999996, 0.3999999998482670627, 0.000000000000000000 ) ) ;
#6364 = ORIENTED_EDGE ( 'NONE', *, *, #17324, .T. ) ;
#6365 = ORIENTED_EDGE ( 'NONE', *, *, #3978, .F. ) ;
#6366 = CARTESIAN_POINT ( 'NONE',  ( -0.3125000000000000000, 0.1294417382415922468, 0.1126388888888907869 ) ) ;
#6367 = CARTESIAN_POINT ( 'NONE',  ( 0.2206173157302028787, 3.911888889040621375, 0.2206173157302027954 ) ) ;
#6368 = CARTESIAN_POINT ( 'NONE',  ( 0.05455304208337304755, -0.2715891510243326756, 0.3880822748423150559 ) ) ;
#6369 = TOROIDAL_SURFACE ( 'NONE', #23096, 0.2510000000000000009, 0.0009999999999999896125 ) ;
#6370 = ORIENTED_EDGE ( 'NONE', *, *, #7809, .T. ) ;
#6371 = ADVANCED_FACE ( 'NONE', ( #918 ), #12040, .T. ) ;
#6372 = APPROVAL_DATE_TIME ( #4900, #11811 ) ;
#6373 = EDGE_CURVE ( 'NONE', #16983, #9622, #11487, .T. ) ;
#6374 = CARTESIAN_POINT ( 'NONE',  ( 0.3125000000000000000, 3.827021247335477694E-17, 1.326383476483184332 ) ) ;
#6375 = CARTESIAN_POINT ( 'NONE',  ( -0.2934963008899025283, 4.999115531676239677, -0.1058924737439701086 ) ) ;
#6376 = ORIENTED_EDGE ( 'NONE', *, *, #12032, .F. ) ;
#6377 = CARTESIAN_POINT ( 'NONE',  ( 0.1167790944451423535, 0.09444444436857780956, 0.2819296736111110424 ) ) ;
#6378 = VERTEX_POINT ( 'NONE', #21165 ) ;
#6379 = CARTESIAN_POINT ( 'NONE',  ( 0.2200028038784669626, 4.259231549017496121, -0.2224089350982841329 ) ) ;
#6380 = CARTESIAN_POINT ( 'NONE',  ( 0.1380212367034616694, 0.4615792792006457312, 0.4105854900893666781 ) ) ;
#6381 = FACE_OUTER_BOUND ( 'NONE', #11749, .T. ) ;
#6382 = CARTESIAN_POINT ( 'NONE',  ( -0.1116596296178200276, 0.1866071427596004417, 0.3436530038418508792 ) ) ;
#6383 = DIRECTION ( 'NONE',  ( -0.5773502691896258421, -0.5773502691896258421, -0.5773502691896258421 ) ) ;
#6384 = CARTESIAN_POINT ( 'NONE',  ( -0.2233192592356399442, 0.3937499999024575148, -0.3073725909049499494 ) ) ;
#6385 = CARTESIAN_POINT ( 'NONE',  ( -0.3236067977499789694, 0.1339285712334866152, -0.2351141009169893104 ) ) ;
#6386 = CIRCLE ( 'NONE', #20017, 0.2109499999999998043 ) ;
#6387 = CARTESIAN_POINT ( 'NONE',  ( 5.178964085587577574E-17, 5.213972222298088433, 0.2819296736111110979 ) ) ;
#6388 = CARTESIAN_POINT ( 'NONE',  ( 0.000000000000000000, 0.02999999999999995379, -0.3125000000000000000 ) ) ;
#6389 = CARTESIAN_POINT ( 'NONE',  ( -0.2200173413850973203, 5.171548481154046861, -0.1982843659929367508 ) ) ;
#6390 = DIRECTION ( 'NONE',  ( 0.000000000000000000, 0.000000000000000000, -1.000000000000000000 ) ) ;
#6391 = CARTESIAN_POINT ( 'NONE',  ( 0.3119999999999999996, 4.588972222373954857, -0.1292346314604056745 ) ) ;
#6392 = CARTESIAN_POINT ( 'NONE',  ( -0.2819296736111110424, 4.870222222298087544, 0.1167790944451424923 ) ) ;
#6393 = ORIENTED_EDGE ( 'NONE', *, *, #828, .T. ) ;
#6394 = CARTESIAN_POINT ( 'NONE',  ( 5.178964085587577574E-17, 4.088972222298087544, 0.2819296736111110979 ) ) ;
#6395 = ORIENTED_EDGE ( 'NONE', *, *, #21398, .F. ) ;
#6396 = CARTESIAN_POINT ( 'NONE',  ( 0.3613381517857143232, 0.2794642856167433020, 0.000000000000000000 ) ) ;
#6397 = ORIENTED_EDGE ( 'NONE', *, *, #23603, .T. ) ;
#6398 = ORIENTED_EDGE ( 'NONE', *, *, #6916, .T. ) ;
#6399 = COORDINATED_UNIVERSAL_TIME_OFFSET ( 0, 0, .AHEAD. ) ;
#6400 = VECTOR ( 'NONE', #5649, 39.37007874015748143 ) ;
#6401 = EDGE_CURVE ( 'NONE', #12731, #18304, #13211, .T. ) ;
#6402 = CARTESIAN_POINT ( 'NONE',  ( 0.3125000000000000000, -5.740531871003217465E-17, 0.03972222222222387966 ) ) ;
#6403 = CARTESIAN_POINT ( 'NONE',  ( -0.3125000000000000000, 1.913510623667739771E-17, 0.2827777777777810142 ) ) ;
#6404 = CARTESIAN_POINT ( 'NONE',  ( 0.4593750000000002554, -1.978974282089605735E-13, 0.4343810118395207698 ) ) ;
#6405 = CARTESIAN_POINT ( 'NONE',  ( 0.2077910874648161710, 5.154453376781931162, -0.2182455333876957004 ) ) ;
#6406 = CARTESIAN_POINT ( 'NONE',  ( -0.4593748724839620823, -0.02270121287663673382, 0.4343774780089812437 ) ) ;
#6407 = CARTESIAN_POINT ( 'NONE',  ( -0.4687500000000002776, -0.04411484026395268848, 0.4171991399623933838 ) ) ;
#6408 = AXIS2_PLACEMENT_3D ( 'NONE', #14899, #11000, #20143 ) ;
#6409 = CARTESIAN_POINT ( 'NONE',  ( -5.731347020009612645E-17, 0.2194444442927115380, 0.3119999999999999996 ) ) ;
#6410 = CARTESIAN_POINT ( 'NONE',  ( 0.1993543840281266910, 0.09791666659080001944, -0.1993543840281266910 ) ) ;
#6411 = CARTESIAN_POINT ( 'NONE',  ( 0.2764156081756483641, -0.1144950937579611167, 0.001527777777778965927 ) ) ;
#6412 = CARTESIAN_POINT ( 'NONE',  ( 1.998815303304990465, 2.291712385858714729, -2.661240473580836152 ) ) ;
#6413 = CARTESIAN_POINT ( 'NONE',  ( -0.2819296736111110979, 4.630638888964754507, 0.000000000000000000 ) ) ;
#6414 = CARTESIAN_POINT ( 'NONE',  ( -0.2800968539712042626, 1.715098578335394762E-17, -0.06926352063787094560 ) ) ;
#6415 = CARTESIAN_POINT ( 'NONE',  ( -0.3048832246468780593, 0.3952586090242287686, -1.145453902462662432 ) ) ;
#6416 = DIRECTION ( 'NONE',  ( -0.7705154201994630636, 1.803387422376048611E-06, -0.6374213576839050654 ) ) ;
#6417 = DIRECTION ( 'NONE',  ( -0.000000000000000000, 0.2588190451025213501, -0.9659258262890680902 ) ) ;
#6418 = CARTESIAN_POINT ( 'NONE',  ( 0.3119999999999999996, 4.297305555555554157, 0.1292346314604056190 ) ) ;
#6419 = CARTESIAN_POINT ( 'NONE',  ( 0.000000000000000000, 0.3125000000000000000, 0.1577777777777800150 ) ) ;
#6420 = AXIS2_PLACEMENT_3D ( 'NONE', #7755, #18977, #11666 ) ;
#6421 = CARTESIAN_POINT ( 'NONE',  ( 0.02036188714951491646, 4.961035658764420653, 0.3119999977765351429 ) ) ;
#6422 = DIRECTION ( 'NONE',  ( 8.659560562354932858E-17, 0.7071067811865474617, -0.7071067811865474617 ) ) ;
#6423 = VERTEX_POINT ( 'NONE', #10203 ) ;
#6424 = DIRECTION ( 'NONE',  ( -0.000000000000000000, -0.000000000000000000, -1.000000000000000000 ) ) ;
#6425 = ORIENTED_EDGE ( 'NONE', *, *, #17974, .T. ) ;
#6426 = CC_DESIGN_DATE_AND_TIME_ASSIGNMENT ( #8527, #19508, ( #1033 ) ) ;
#6427 = CARTESIAN_POINT ( 'NONE',  ( 0.05605008125374450617, 4.684288922465986715, 0.3069347663937170845 ) ) ;
#6428 = CARTESIAN_POINT ( 'NONE',  ( 0.3950000000000000178, 0.05000000000000028727, -2.591000000000000192 ) ) ;
#6429 = CARTESIAN_POINT ( 'NONE',  ( 0.3155070326520292845, -5.795770164686806123E-17, 0.1490972222222247956 ) ) ;
#6430 = AXIS2_PLACEMENT_3D ( 'NONE', #1877, #4183, #6007 ) ;
#6431 = CARTESIAN_POINT ( 'NONE',  ( -1.910449006669871087E-17, 4.425777777777777366, -0.3119999999999999996 ) ) ;
#6432 = ORIENTED_EDGE ( 'NONE', *, *, #19371, .T. ) ;
#6433 = CARTESIAN_POINT ( 'NONE',  ( -0.2923287055106771337, -0.03482142866897096345, 0.2123892367102619971 ) ) ;
#6434 = CARTESIAN_POINT ( 'NONE',  ( 1.726321361862525858E-17, 0.06319444436857780956, -0.2819296736111110979 ) ) ;
#6435 = CARTESIAN_POINT ( 'NONE',  ( -0.1144950937579609779, 0.2764156081756484196, 0.02930555555555695163 ) ) ;
#6436 = DIRECTION ( 'NONE',  ( 0.000000000000000000, 1.000000000000000000, 0.000000000000000000 ) ) ;
#6437 = CARTESIAN_POINT ( 'NONE',  ( 0.2206173157302027676, 0.5111111111111107386, 0.2206173157302028787 ) ) ;
#6438 = FACE_OUTER_BOUND ( 'NONE', #17793, .T. ) ;
#6439 = EDGE_LOOP ( 'NONE', ( #8671, #24112 ) ) ;
#6440 = CARTESIAN_POINT ( 'NONE',  ( -1.062695237341364068E-12, 5.118312382271687611, 0.3086920601714014945 ) ) ;
#6441 = EDGE_CURVE ( 'NONE', #2791, #23806, #13975, .T. ) ;
#6442 = CARTESIAN_POINT ( 'NONE',  ( -0.3105867304364036685, 4.281119371102881210, 0.04220986312590439132 ) ) ;
#6443 = LOCAL_TIME ( 21, 9, 13.00000000000000000, #6003 ) ;
#6444 = FACE_OUTER_BOUND ( 'NONE', #15190, .T. ) ;
#6445 = CARTESIAN_POINT ( 'NONE',  ( 0.3119999999999999996, 0.5736111111111107386, 0.000000000000000000 ) ) ;
#6446 = CARTESIAN_POINT ( 'NONE',  ( 0.3119999999999999996, 4.915361111111109516, -0.1292346314604056745 ) ) ;
#6447 = CARTESIAN_POINT ( 'NONE',  ( 0.1167790944451422702, 4.016055555631422358, -0.2819296736111110424 ) ) ;
#6448 = CARTESIAN_POINT ( 'NONE',  ( -0.1292346314604056190, 0.5840277776260448528, -0.3119999999999999996 ) ) ;
#6449 = CARTESIAN_POINT ( 'NONE',  ( -0.4500000000000003997, 0.2598076211353315124, 0.3779506566538943790 ) ) ;
#6450 = CARTESIAN_POINT ( 'NONE',  ( 0.3614195271177944591, -9.204707668395282654E-18, -0.008981461429929990525 ) ) ;
#6451 = EDGE_LOOP ( 'NONE', ( #6432, #4024, #1251, #17987, #52, #6280, #15549 ) ) ;
#6452 = ORIENTED_EDGE ( 'NONE', *, *, #2001, .F. ) ;
#6453 = CARTESIAN_POINT ( 'NONE',  ( -0.3124999999999989453, 0.1294417382415933293, 0.1195833333333356230 ) ) ;
#6454 = CARTESIAN_POINT ( 'NONE',  ( 0.1167790944451422702, 4.668833333409200037, -0.2819296736111110424 ) ) ;
#6455 = EDGE_CURVE ( 'NONE', #22264, #175, #1419, .T. ) ;
#6456 = CARTESIAN_POINT ( 'NONE',  ( -0.3613381517857143788, 0.3901785713310290116, 0.1174058825155740310 ) ) ;
#6457 = DIRECTION ( 'NONE',  ( -0.8651979924482607887, 0.04370253788966922681, 0.4995222938423283798 ) ) ;
#6458 = PERSON_AND_ORGANIZATION ( #15518, #2538 ) ;
#6459 = CARTESIAN_POINT ( 'NONE',  ( -0.1144950937579609918, -0.2764156081756484196, -0.06791666666666602847 ) ) ;
#6460 = LOCAL_TIME ( 21, 9, 13.00000000000000000, #20382 ) ;
#6461 = CARTESIAN_POINT ( 'NONE',  ( 0.2819296736111110979, 4.286888888964754507, -0.1167790944451423396 ) ) ;
#6462 = CARTESIAN_POINT ( 'NONE',  ( -0.2993258702403846505, 4.832972278583333114, -0.09025194431095438785 ) ) ;
#6463 = FACE_OUTER_BOUND ( 'NONE', #4802, .T. ) ;
#6464 = CARTESIAN_POINT ( 'NONE',  ( -0.2764156081756484196, -0.1144950937579609362, 0.09875000000000193345 ) ) ;
#6465 = LINE ( 'NONE', #8290, #7540 ) ;
#6466 = CARTESIAN_POINT ( 'NONE',  ( 1.726321361862525858E-17, 0.6187499999241333759, -0.2819296736111110979 ) ) ;
#6467 = DIRECTION ( 'NONE',  ( -0.5850251379555668763, 0.7373335635563863510, 0.3377644208813451177 ) ) ;
#6468 = DIRECTION ( 'NONE',  ( -0.000000000000000000, -1.000000000000000000, -0.000000000000000000 ) ) ;
#6469 = CARTESIAN_POINT ( 'NONE',  ( 0.3236067977499789694, 0.3928571428571427382, 0.2351141009169893659 ) ) ;
#6470 = CARTESIAN_POINT ( 'NONE',  ( 0.3155070326520292290, -0.1306872919485616569, 0.4754861111111158278 ) ) ;
#6471 = DIRECTION ( 'NONE',  ( 0.000000000000000000, 0.000000000000000000, 1.000000000000000000 ) ) ;
#6472 = EDGE_CURVE ( 'NONE', #5016, #4599, #3999, .T. ) ;
#6473 = DIRECTION ( 'NONE',  ( 0.000000000000000000, -0.9961946980917454342, 0.08715574274765829077 ) ) ;
#6474 = CARTESIAN_POINT ( 'NONE',  ( -0.1993543840281266633, 0.3895833332574667462, -0.1993543840281266910 ) ) ;
#6475 = CARTESIAN_POINT ( 'NONE',  ( -5.178964085587577574E-17, 0.4104166665908000056, 0.2819296736111110979 ) ) ;
#6476 = EDGE_CURVE ( 'NONE', #787, #5016, #11671, .T. ) ;
#6477 = EDGE_CURVE ( 'NONE', #769, #16532, #12421, .T. ) ;
#6478 = CARTESIAN_POINT ( 'NONE',  ( 0.1167790944451422702, 4.127166666742532186, -0.2819296736111110424 ) ) ;
#6479 = CARTESIAN_POINT ( 'NONE',  ( -0.1236067977499790416, 0.3696428569477723247, 0.3804226065180614236 ) ) ;
#6480 = CARTESIAN_POINT ( 'NONE',  ( -0.2819296736111110424, 4.759111111186978604, 0.1167790944451424923 ) ) ;
#6481 = CARTESIAN_POINT ( 'NONE',  ( 0.2754369701929059167, 5.127252903595911349, 0.1376149775922576313 ) ) ;
#6482 = CARTESIAN_POINT ( 'NONE',  ( 0.2206173157302028232, 0.4069444442927114824, -0.2206173157302028232 ) ) ;
#6483 = SECURITY_CLASSIFICATION ( '', '', #17084 ) ;
#6484 = ORIENTED_EDGE ( 'NONE', *, *, #9456, .T. ) ;
#6485 = ORIENTED_EDGE ( 'NONE', *, *, #11537, .F. ) ;
#6486 = CARTESIAN_POINT ( 'NONE',  ( 0.2206173157302027954, 4.696611111111110404, -0.2206173157302028232 ) ) ;
#6487 = CARTESIAN_POINT ( 'NONE',  ( 0.1292346314604056190, 3.929250000151732536, -0.3119999999999999996 ) ) ;
#6488 = EDGE_CURVE ( 'NONE', #6278, #2537, #20887, .T. ) ;
#6489 = CARTESIAN_POINT ( 'NONE',  ( 0.009375000000000065573, -0.5358532185916218271, 0.3779506566538943235 ) ) ;
#6490 = AXIS2_PLACEMENT_3D ( 'NONE', #14384, #12938, #21811 ) ;
#6491 =( BOUNDED_SURFACE ( )  B_SPLINE_SURFACE ( 3, 2, ( 
 ( #3598, #18240, #1772 ),
 ( #7028, #20431, #1894 ),
 ( #1539, #8971, #23828 ),
 ( #14590, #9337, #16773 ),
 ( #57, #15185, #2262 ),
 ( #9696, #19077, #19320 ),
 ( #7741, #2385, #13491 ),
 ( #7621, #11901, #181 ),
 ( #4076, #11407, #22854 ),
 ( #18965, #301, #9821 ),
 ( #6267, #2619, #15306 ),
 ( #11772, #13253, #8089 ) ),
 .UNSPECIFIED., .F., .F., .T. ) 
 B_SPLINE_SURFACE_WITH_KNOTS ( ( 4, 2, 2, 2, 2, 4 ),
 ( 3, 3 ),
 ( 0.03744456216066675835, 0.04077857935059427813, 0.04244558794555804149, 0.04411259654052179791, 0.04744661373044932462, 0.05078063092037684439 ),
 ( 0.000000000000000000, 1.000000000000000000 ),
 .UNSPECIFIED. ) 
 GEOMETRIC_REPRESENTATION_ITEM ( )  RATIONAL_B_SPLINE_SURFACE ( (
 ( 1.000000000000000000, 0.8464669816041904271, 1.000000000000000000),
 ( 1.000000000000000000, 0.8515868425021679844, 1.000000000000000000),
 ( 1.000000000000000000, 0.8564835659291879510, 1.000000000000000000),
 ( 1.000000000000000000, 0.8619139284918067023, 1.000000000000000000),
 ( 1.000000000000000000, 0.8633991495534405480, 1.000000000000000000),
 ( 1.000000000000000000, 0.8654490525000912982, 1.000000000000000000),
 ( 1.000000000000000000, 0.8660089163969103554, 1.000000000000000000),
 ( 1.000000000000000000, 0.8660572738274423532, 1.000000000000000000),
 ( 1.000000000000000000, 0.8638780250325636123, 1.000000000000000000),
 ( 1.000000000000000000, 0.8566598902920686820, 1.000000000000000000),
 ( 1.000000000000000000, 0.8517009389554219823, 1.000000000000000000),
 ( 1.000000000000000000, 0.8464669816041900940, 1.000000000000000000) ) ) 
 REPRESENTATION_ITEM ( '' )  SURFACE ( )  );
#6492 =( BOUNDED_SURFACE ( )  B_SPLINE_SURFACE ( 3, 2, ( 
 ( #14563, #9189, #3822 ),
 ( #1511, #20288, #14925 ),
 ( #22344, #16394, #3573 ),
 ( #5646, #11026, #13111 ),
 ( #20525, #11265, #1992 ),
 ( #7123, #12751, #20166 ),
 ( #3453, #16511, #23925 ),
 ( #2359, #15641, #2596 ),
 ( #15280, #2239, #9799 ),
 ( #18811, #3940, #5998 ) ),
 .UNSPECIFIED., .F., .F., .F. ) 
 B_SPLINE_SURFACE_WITH_KNOTS ( ( 4, 2, 2, 2, 4 ),
 ( 3, 3 ),
 ( 0.04463809143445898048, 0.04796255359614957914, 0.05128701575784017086, 0.05461147791953076258, 0.05793594008122135430 ),
 ( 0.000000000000000000, 1.000000000000000000 ),
 .UNSPECIFIED. ) 
 GEOMETRIC_REPRESENTATION_ITEM ( )  RATIONAL_B_SPLINE_SURFACE ( (
 ( 1.000000000000000000, 0.8285407536241361504, 1.000000000000000000),
 ( 1.000000000000000000, 0.8326168960428312893, 1.000000000000000000),
 ( 1.000000000000000000, 0.8363786027323962813, 1.000000000000000000),
 ( 1.000000000000000000, 0.8417912930207285260, 1.000000000000000000),
 ( 1.000000000000000000, 0.8433923807916883231, 1.000000000000000000),
 ( 1.000000000000000000, 0.8433905099817204931, 1.000000000000000000),
 ( 1.000000000000000000, 0.8417888685870387189, 1.000000000000000000),
 ( 1.000000000000000000, 0.8363766775001262310, 1.000000000000000000),
 ( 1.000000000000000000, 0.8326159398061623307, 1.000000000000000000),
 ( 1.000000000000000000, 0.8285407536241354842, 1.000000000000000000) ) ) 
 REPRESENTATION_ITEM ( '' )  SURFACE ( )  );
#6493 = CALENDAR_DATE ( 2026, 7, 10 ) ;
#6494 = ORIENTED_EDGE ( 'NONE', *, *, #4412, .T. ) ;
#6495 = FACE_OUTER_BOUND ( 'NONE', #2880, .T. ) ;
#6496 = ADVANCED_FACE ( 'NONE', ( #23334 ), #14093, .F. ) ;
#6497 = CARTESIAN_POINT ( 'NONE',  ( 0.2206173157302028232, 0.2472222222222218435, -0.2206173157302028232 ) ) ;
#6498 = ORIENTED_EDGE ( 'NONE', *, *, #17202, .F. ) ;
#6499 = CARTESIAN_POINT ( 'NONE',  ( 0.1167790944451423257, 0.1152777777019111521, -0.2819296736111110424 ) ) ;
#6500 = CARTESIAN_POINT ( 'NONE',  ( 0.2821852889849572610, 4.256074823217026015, -0.1331099846749929372 ) ) ;
#6501 = CARTESIAN_POINT ( 'NONE',  ( -0.2206173157302028787, 0.3305555555555552139, 0.2206173157302027954 ) ) ;
#6502 = CARTESIAN_POINT ( 'NONE',  ( 0.3018349262019693890, 4.083264140120535401, 0.07899231521169805537 ) ) ;
#6503 = CARTESIAN_POINT ( 'NONE',  ( 2.326421213736078119E-17, 0.3687499999024574371, -0.3799334167787516425 ) ) ;
#6504 = DIRECTION ( 'NONE',  ( -0.000000000000000000, -1.000000000000000000, -0.000000000000000000 ) ) ;
#6505 = LINE ( 'NONE', #4915, #23629 ) ;
#6506 = CIRCLE ( 'NONE', #17408, 0.7199999999999994182 ) ;
#6507 = ORIENTED_EDGE ( 'NONE', *, *, #14381, .F. ) ;
#6508 = CARTESIAN_POINT ( 'NONE',  ( -0.1912962694986284351, 4.660659591632862586, -0.2498291629754902654 ) ) ;
#6509 = B_SPLINE_CURVE_WITH_KNOTS ( 'NONE', 3,
 ( #6414, #13868, #12048, #2171, #2290, #9604, #17035, #15212, #22647, #20815, #4105, #11564, #9725, #17161, #451, #7882, #22762, #3121, #10330, #10453, #6775, #23586, #2871, #12170, #6903, #21893, #14219, #19461, #12407, #21656, #18121, #17880, #14101, #10572, #16051, #10687, #4702, #16293, #2759, #1418, #8720, #10210, #14341, #18003 ),
 .UNSPECIFIED., .F., .F.,
 ( 4, 2, 1, 2, 2, 2, 2, 2, 2, 1, 2, 2, 2, 2, 2, 2, 2, 2, 2, 2, 2, 2, 4 ),
 ( 0.004595939250185037024, 0.005313238532186213142, 0.006030537814187388393, 0.006747837096188564511, 0.007465136378189738894, 0.008899734942192091131, 0.01033433350619443990, 0.01176893207019679040, 0.01248623135219796565, 0.01320353063419914263, 0.01392082991620031962, 0.01463812919820149661, 0.01607272776220385058, 0.01750732632620620455, 0.01894192489020856199, 0.01965922417220973550, 0.02037652345421091249, 0.02181112201821325952, 0.02324572058221561002, 0.02396301986421678354, 0.02468031914621796052, 0.02611491771022031103, 0.02754951627422265806 ),
 .UNSPECIFIED. ) ;
#6510 = CARTESIAN_POINT ( 'NONE',  ( 0.1167790944451424368, 3.870222222298087988, 0.2819296736111110424 ) ) ;
#6511 = CARTESIAN_POINT ( 'NONE',  ( -8.251178249108312710E-07, 5.016022433328296337, 0.3119999999976432181 ) ) ;
#6512 = CARTESIAN_POINT ( 'NONE',  ( -0.2778680883334028184, 5.175875489270271856, -0.09957862134326772585 ) ) ;
#6513 = CARTESIAN_POINT ( 'NONE',  ( -0.2594798065058602776, 4.785276866862929523, 0.1777679019147691830 ) ) ;
#6514 = CARTESIAN_POINT ( 'NONE',  ( -0.1292346314604057023, 4.457027777929509327, 0.3119999999999998885 ) ) ;
#6515 = CARTESIAN_POINT ( 'NONE',  ( -0.1993543840281266355, 4.762583333409199149, 0.1993543840281267465 ) ) ;
#6516 = ORIENTED_EDGE ( 'NONE', *, *, #22890, .F. ) ;
#6517 = CARTESIAN_POINT ( 'NONE',  ( 0.1993543840281266633, 4.165361111186975940, -0.1993543840281266910 ) ) ;
#6518 = ORIENTED_EDGE ( 'NONE', *, *, #10812, .T. ) ;
#6519 = EDGE_LOOP ( 'NONE', ( #6306, #17738, #22618, #15420, #1416 ) ) ;
#6520 = COORDINATED_UNIVERSAL_TIME_OFFSET ( 0, 0, .AHEAD. ) ;
#6521 = CARTESIAN_POINT ( 'NONE',  ( 2.094306190944884349, 2.923228049659837069, -2.986000000000000210 ) ) ;
#6522 = CARTESIAN_POINT ( 'NONE',  ( 0.2206173157302027676, 0.4555555555555552139, 0.2206173157302028787 ) ) ;
#6523 = CARTESIAN_POINT ( 'NONE',  ( 0.4593750000000006994, 0.04451021669580589035, 0.4343810118395315389 ) ) ;
#6524 = B_SPLINE_CURVE_WITH_KNOTS ( 'NONE', 3,
 ( #10410, #4659, #23295, #1003, #17470, #6608, #14173, #23536, #17590, #21604, #12360, #21253, #19778, #3076, #17952, #12003, #881, #3548 ),
 .UNSPECIFIED., .F., .F.,
 ( 4, 2, 2, 2, 2, 2, 2, 2, 4 ),
 ( 1.514782153580211930E-17, 0.001110697466041064363, 0.002221394932082113548, 0.003332092398123162515, 0.004442789864164211483, 0.005553487330205260884, 0.006664184796246309418, 0.007774882262287358820, 0.008885579728328409088 ),
 .UNSPECIFIED. ) ;
#6525 = CARTESIAN_POINT ( 'NONE',  ( 0.000000000000000000, 0.4997679491924311157, -0.3125000000000001665 ) ) ;
#6526 = CARTESIAN_POINT ( 'NONE',  ( -0.4593400809164812082, -0.04533910969798598395, 0.4334227803821231184 ) ) ;
#6527 = LINE ( 'NONE', #4695, #6165 ) ;
#6528 = CARTESIAN_POINT ( 'NONE',  ( 0.2084225359521126864, -0.1824881659814967805, 0.3875005808676508789 ) ) ;
#6529 = CARTESIAN_POINT ( 'NONE',  ( 0.2819296736111110979, 0.09097222214635558579, 0.000000000000000000 ) ) ;
#6530 = CARTESIAN_POINT ( 'NONE',  ( 0.1144950937579611444, 0.2764156081756483641, -0.04013888888888803713 ) ) ;
#6531 = DIRECTION ( 'NONE',  ( -0.000000000000000000, -1.000000000000000000, -0.000000000000000000 ) ) ;
#6532 = CARTESIAN_POINT ( 'NONE',  ( -0.1167790944451423535, 4.418833333409198261, 0.2819296736111110424 ) ) ;
#6533 = CARTESIAN_POINT ( 'NONE',  ( 0.1092791156175890038, 5.203332556872312331, 0.2819296736111110424 ) ) ;
#6534 = CARTESIAN_POINT ( 'NONE',  ( -0.1836571724648604909, 0.7278005416041625208, -1.080755778418241109 ) ) ;
#6535 = CYLINDRICAL_SURFACE ( 'NONE', #14137, 0.4000000000000000222 ) ;
#6536 = DIRECTION ( 'NONE',  ( -0.000000000000000000, -1.000000000000000000, -0.000000000000000000 ) ) ;
#6537 = CARTESIAN_POINT ( 'NONE',  ( 0.2206173157302028787, 4.182722222222221120, 0.2206173157302027954 ) ) ;
#6538 = AXIS2_PLACEMENT_3D ( 'NONE', #2440, #17310, #8272 ) ;
#6539 = CARTESIAN_POINT ( 'NONE',  ( -0.3119999999999998885, 5.172305555707287006, 0.1292346314604058410 ) ) ;
#6540 = EDGE_CURVE ( 'NONE', #22476, #6959, #2997, .T. ) ;
#6541 = CARTESIAN_POINT ( 'NONE',  ( 0.1041572415211016039, 4.963483492082001902, 0.2942352266619563395 ) ) ;
#6542 = CYLINDRICAL_SURFACE ( 'NONE', #12886, 0.3125000000000000000 ) ;
#6543 = VERTEX_POINT ( 'NONE', #23458 ) ;
#6544 = CARTESIAN_POINT ( 'NONE',  ( -0.1660923693448534966, 4.882155643265540412, -0.2642717717335951177 ) ) ;
#6545 = CARTESIAN_POINT ( 'NONE',  ( 0.4805070082343984583, -0.2560807851245830435, 0.04413116910601660309 ) ) ;
#6546 = CARTESIAN_POINT ( 'NONE',  ( 0.3155070326520292845, -5.795770164686806123E-17, -0.01756944444444321490 ) ) ;
#6547 = AXIS2_PLACEMENT_3D ( 'NONE', #164, #16642, #7255 ) ;
#6548 = DIRECTION ( 'NONE',  ( -0.000000000000000000, -1.000000000000000000, -0.000000000000000000 ) ) ;
#6549 = VERTEX_POINT ( 'NONE', #6768 ) ;
#6550 = CARTESIAN_POINT ( 'NONE',  ( -0.3613381517857144343, 0.2473214284738860791, 0.1174058825155740171 ) ) ;
#6551 = CARTESIAN_POINT ( 'NONE',  ( -0.1167790944451424506, 0.08749999992413336203, 0.2819296736111110424 ) ) ;
#6552 = CARTESIAN_POINT ( 'NONE',  ( -0.1144950937579609779, 0.2764156081756484196, -0.08180555555555503455 ) ) ;
#6553 = CARTESIAN_POINT ( 'NONE',  ( 0.2209708691207961095, -0.2209708691207961651, 0.4216666666666714081 ) ) ;
#6554 = CARTESIAN_POINT ( 'NONE',  ( -1.515315767888941311E-17, 0.1799999999999999933, -1.242999999999999661 ) ) ;
#6555 = CARTESIAN_POINT ( 'NONE',  ( 0.2764156081756483641, -0.1144950937579611167, 0.4529166666666714636 ) ) ;
#6556 = ORIENTED_EDGE ( 'NONE', *, *, #21909, .F. ) ;
#6557 = DIRECTION ( 'NONE',  ( 0.000000000000000000, 0.000000000000000000, -1.000000000000000000 ) ) ;
#6558 = PRODUCT_RELATED_PRODUCT_CATEGORY ( 'detail', '', ( #12267 ) ) ;
#6559 = CARTESIAN_POINT ( 'NONE',  ( 0.1236067977499789028, 0.09999999999999997780, 0.3804226065180614791 ) ) ;
#6560 = FACE_OUTER_BOUND ( 'NONE', #1347, .T. ) ;
#6561 = CARTESIAN_POINT ( 'NONE',  ( -0.2206173157302027954, 0.4833333333333329485, -0.2206173157302028232 ) ) ;
#6562 = CARTESIAN_POINT ( 'NONE',  ( -0.2206173157302028232, 4.932722222222221120, -0.2206173157302028232 ) ) ;
#6563 = CARTESIAN_POINT ( 'NONE',  ( -0.1993543840281266910, 4.179250000075865223, -0.1993543840281266910 ) ) ;
#6564 = B_SPLINE_CURVE_WITH_KNOTS ( 'NONE', 3,
 ( #2707, #875, #11292, #16889, #9697, #182, #18720, #10158, #20671, #11533 ),
 .UNSPECIFIED., .F., .F.,
 ( 4, 2, 2, 2, 4 ),
 ( 0.000000000000000000, 0.003321633220911225561, 0.006643266441822451122, 0.009964899662733674515, 0.01328653288364489704 ),
 .UNSPECIFIED. ) ;
#6565 = CARTESIAN_POINT ( 'NONE',  ( 0.1993543840281266633, 3.957027777853643791, -0.1993543840281266910 ) ) ;
#6566 = LINE ( 'NONE', #8638, #16661 ) ;
#6567 = CARTESIAN_POINT ( 'NONE',  ( -0.3107848814623954126, 0.3618341423928944645, 0.4134938258000330769 ) ) ;
#6568 = LINE ( 'NONE', #4501, #12601 ) ;
#6569 = ORIENTED_EDGE ( 'NONE', *, *, #11833, .F. ) ;
#6570 = ORIENTED_EDGE ( 'NONE', *, *, #3752, .T. ) ;
#6571 = AXIS2_PLACEMENT_3D ( 'NONE', #1645, #14709, #16529 ) ;
#6572 = CARTESIAN_POINT ( 'NONE',  ( -0.3125000000000000000, 1.913510623667739771E-17, -0.04361111111111011518 ) ) ;
#6573 = CARTESIAN_POINT ( 'NONE',  ( -0.2819296736111110424, 4.523000000075865223, 0.1167790944451424923 ) ) ;
#6574 = CARTESIAN_POINT ( 'NONE',  ( 0.2233192592356400275, 0.004464285616743319737, -0.3073725909049499494 ) ) ;
#6575 = CARTESIAN_POINT ( 'NONE',  ( -0.3119999999999999996, 4.106333333333332725, 0.000000000000000000 ) ) ;
#6576 = APPROVAL_DATE_TIME ( #17561, #3590 ) ;
#6577 = LINE ( 'NONE', #8162, #21649 ) ;
#6578 = CARTESIAN_POINT ( 'NONE',  ( 0.2764156081756483641, -0.1144950937579611167, -0.05402777777777704321 ) ) ;
#6579 = CARTESIAN_POINT ( 'NONE',  ( 1.020000000000000018, 2.665000000000000036, -2.591000000000000192 ) ) ;
#6580 = CARTESIAN_POINT ( 'NONE',  ( -0.2819296736111110979, 4.085500000075865223, -0.1167790944451422980 ) ) ;
#6581 = APPROVAL_DATE_TIME ( #15971, #10761 ) ;
#6582 = SPHERICAL_SURFACE ( 'NONE', #21617, 0.3119999999999999996 ) ;
#6583 = PLANE ( 'NONE',  #18307 ) ;
#6584 = CARTESIAN_POINT ( 'NONE',  ( -0.1954553509668046918, -0.1954553509668046640, 0.1577777777777801815 ) ) ;
#6585 = CARTESIAN_POINT ( 'NONE',  ( 0.2233192592356399164, 0.0008928570453147456013, 0.3073725909049500604 ) ) ;
#6586 = CARTESIAN_POINT ( 'NONE',  ( -0.1167790944451422702, 0.1083333332574667046, -0.2819296736111110424 ) ) ;
#6587 = CARTESIAN_POINT ( 'NONE',  ( -0.2523926463571780632, 0.1523216146538590721, 0.4063109944092492820 ) ) ;
#6588 = CARTESIAN_POINT ( 'NONE',  ( -0.1292346314604058410, 0.4451388888888885287, 0.3119999999999998885 ) ) ;
#6589 = DIRECTION ( 'NONE',  ( 0.000000000000000000, -0.000000000000000000, 1.000000000000000000 ) ) ;
#6590 = DIRECTION ( 'NONE',  ( -1.000000000000000000, 0.000000000000000000, 0.000000000000000000 ) ) ;
#6591 = CARTESIAN_POINT ( 'NONE',  ( 0.3155070326520292845, -5.795770164686806123E-17, 0.4789583333333381487 ) ) ;
#6592 = EDGE_CURVE ( 'NONE', #19405, #70, #14904, .T. ) ;
#6593 = CARTESIAN_POINT ( 'NONE',  ( 0.3120000000000000551, 3.963972222222221564, 0.1292346314604056190 ) ) ;
#6594 = CARTESIAN_POINT ( 'NONE',  ( -0.3120015917345935752, 3.781041443398025059, 0.04082955656978376480 ) ) ;
#6595 = CARTESIAN_POINT ( 'NONE',  ( -0.2494961085522761357, 3.841226936246323831, 0.1917385093088717907 ) ) ;
#6596 = CARTESIAN_POINT ( 'NONE',  ( 1.726321361862525858E-17, 0.3826388888130222710, -0.2819296736111110979 ) ) ;
#6597 = CARTESIAN_POINT ( 'NONE',  ( 0.1993543840281266633, 4.123694444520309865, -0.1993543840281266910 ) ) ;
#6598 = CARTESIAN_POINT ( 'NONE',  ( 0.1116596296178199027, -0.002678571526113819427, 0.3436530038418508792 ) ) ;
#6599 = B_SPLINE_CURVE_WITH_KNOTS ( 'NONE', 3,
 ( #22255, #7386, #14952, #11050, #5673, #20314, #9088, #10932, #20551, #5183, #12898, #22372, #11291, #7504, #2018, #23956, #16656, #5311, #12654, #18360, #12775, #18479 ),
 .UNSPECIFIED., .F., .F.,
 ( 4, 2, 2, 2, 2, 2, 2, 2, 2, 2, 4 ),
 ( 0.002245614500282211434, 0.002912534838767885485, 0.003579455177253559536, 0.004913295854224907638, 0.006247136531196254873, 0.007580977208167602975, 0.008914817885138950210, 0.009581738223624625128, 0.01024865856211029831, 0.01158249923908164641, 0.01291633991605299452 ),
 .UNSPECIFIED. ) ;
#6600 = CARTESIAN_POINT ( 'NONE',  ( -0.1167790944451423257, 4.745222222298088433, -0.2819296736111110424 ) ) ;
#6601 = CARTESIAN_POINT ( 'NONE',  ( 0.2303917398207527556, 5.125144739340170119, 0.2040722439002406741 ) ) ;
#6602 = DIRECTION ( 'NONE',  ( 0.000000000000000000, 0.000000000000000000, 1.000000000000000000 ) ) ;
#6603 = ORIENTED_EDGE ( 'NONE', *, *, #9517, .T. ) ;
#6604 = CARTESIAN_POINT ( 'NONE',  ( 0.000000000000000000, 0.3125000000000000000, 0.3869444444444488651 ) ) ;
#6605 = CARTESIAN_POINT ( 'NONE',  ( -0.3119999999999998885, 3.838972222373954857, 0.1292346314604058410 ) ) ;
#6606 = LINE ( 'NONE', #15522, #18470 ) ;
#6607 = AXIS2_PLACEMENT_3D ( 'NONE', #17949, #878, #13937 ) ;
#6608 = CARTESIAN_POINT ( 'NONE',  ( 0.2161795966814163694, 0.03242967361111068897, 0.1815435138465212317 ) ) ;
#6609 = CARTESIAN_POINT ( 'NONE',  ( -0.2819296736111110979, 4.793833333409199149, -0.1167790944451422980 ) ) ;
#6610 = CALENDAR_DATE ( 2026, 7, 10 ) ;
#6611 = VERTEX_POINT ( 'NONE', #11282 ) ;
#6612 = CARTESIAN_POINT ( 'NONE',  ( -0.05041081173230543833, 5.101548709612324650, -0.3067424804290312945 ) ) ;
#6613 = EDGE_LOOP ( 'NONE', ( #8129, #10426, #16240, #10292 ) ) ;
#6614 = CARTESIAN_POINT ( 'NONE',  ( 0.3119999999999999996, 0.6256944442927115935, -0.1292346314604056468 ) ) ;
#6615 = CARTESIAN_POINT ( 'NONE',  ( 2.781172880863639385E-17, 6.000000000000000888, 0.2041999999999999926 ) ) ;
#6616 = CARTESIAN_POINT ( 'NONE',  ( -0.3119999999999999996, 0.3201388888888885287, -0.1292346314604056745 ) ) ;
#6617 = CARTESIAN_POINT ( 'NONE',  ( 0.3011242999017837985, 4.083187727495992903, 0.08166723430258095162 ) ) ;
#6618 = CARTESIAN_POINT ( 'NONE',  ( -0.1116596296178199582, 0.2294642856167432854, -0.3436530038418508792 ) ) ;
#6619 = CARTESIAN_POINT ( 'NONE',  ( -0.2620971190287328390, 5.062880408242417474, 0.1705199924471070549 ) ) ;
#6620 = EDGE_CURVE ( 'NONE', #6190, #22559, #3956, .T. ) ;
#6621 = AXIS2_PLACEMENT_3D ( 'NONE', #19870, #3162, #4987 ) ;
#6622 = CARTESIAN_POINT ( 'NONE',  ( 2.168722887430706070, 2.291712385858714729, -1.763529041877836212 ) ) ;
#6623 = AXIS2_PLACEMENT_3D ( 'NONE', #9176, #14801, #18563 ) ;
#6624 = CARTESIAN_POINT ( 'NONE',  ( -3.990790521751304672E-07, 4.654944455680286808, -0.3119999999997447038 ) ) ;
#6625 = CARTESIAN_POINT ( 'NONE',  ( -0.1167790944451423257, 3.786888888964754063, -0.2819296736111110424 ) ) ;
#6626 = LINE ( 'NONE', #15660, #4777 ) ;
#6627 = FACE_OUTER_BOUND ( 'NONE', #21211, .T. ) ;
#6628 = CARTESIAN_POINT ( 'NONE',  ( -0.1535721704690733991, 4.770579318579037498, -0.2744936891675854862 ) ) ;
#6629 = CARTESIAN_POINT ( 'NONE',  ( -0.2206173157302027676, 4.509111111262843252, 0.2206173157302028787 ) ) ;
#6630 = CARTESIAN_POINT ( 'NONE',  ( 5.178964085587577574E-17, 4.769527777853643791, 0.2819296736111110979 ) ) ;
#6631 = ORIENTED_EDGE ( 'NONE', *, *, #9929, .T. ) ;
#6632 = EDGE_CURVE ( 'NONE', #19164, #14671, #18471, .T. ) ;
#6633 = CARTESIAN_POINT ( 'NONE',  ( -0.2819296736111110979, 4.130638888964754507, 0.000000000000000000 ) ) ;
#6634 = ORIENTED_EDGE ( 'NONE', *, *, #2627, .T. ) ;
#6635 = ORIENTED_EDGE ( 'NONE', *, *, #935, .T. ) ;
#6636 = TOROIDAL_SURFACE ( 'NONE', #18702, 0.2510000000000000009, 0.001000000000000037101 ) ;
#6637 = EDGE_CURVE ( 'NONE', #18060, #3289, #3716, .T. ) ;
#6638 = AXIS2_PLACEMENT_3D ( 'NONE', #22724, #2124, #20897 ) ;
#6639 = EDGE_CURVE ( 'NONE', #15989, #9981, #15113, .T. ) ;
#6640 = COORDINATED_UNIVERSAL_TIME_OFFSET ( 0, 0, .AHEAD. ) ;
#6641 = CARTESIAN_POINT ( 'NONE',  ( 0.4687500000000003886, 0.2598076211353211318, 0.06112444011295851964 ) ) ;
#6642 = CARTESIAN_POINT ( 'NONE',  ( 0.2730879860166738338, 4.111524471938507119, -3.027594437230249902 ) ) ;
#6643 = CARTESIAN_POINT ( 'NONE',  ( 1.910449006669871087E-17, 0.02499999984826707308, -0.3119999999999999996 ) ) ;
#6644 = CARTESIAN_POINT ( 'NONE',  ( -0.1825813392756855669, 4.382625187681782108, -0.2540029803607526948 ) ) ;
#6645 = DIRECTION ( 'NONE',  ( -0.000000000000000000, 1.000000000000000000, -0.000000000000000000 ) ) ;
#6646 = CARTESIAN_POINT ( 'NONE',  ( 0.1312456515338671081, 0.1993400706575450265, -0.7385206977513997240 ) ) ;
#6647 = EDGE_CURVE ( 'NONE', #11791, #8318, #15525, .T. ) ;
#6648 = ORIENTED_EDGE ( 'NONE', *, *, #11423, .F. ) ;
#6649 = ORIENTED_EDGE ( 'NONE', *, *, #7479, .T. ) ;
#6650 = CARTESIAN_POINT ( 'NONE',  ( -0.1144950937579609779, 0.2764156081756484196, 0.3556944444444484765 ) ) ;
#6651 = CARTESIAN_POINT ( 'NONE',  ( 0.1167790944451423119, 0.04583333325746669767, -0.2819296736111110979 ) ) ;
#6652 = CARTESIAN_POINT ( 'NONE',  ( 0.1144950937579611444, 0.2764156081756483641, 0.1265277777777799595 ) ) ;
#6653 = CARTESIAN_POINT ( 'NONE',  ( -0.1167790944451423257, 4.453555555631420582, -0.2819296736111110424 ) ) ;
#6654 = CARTESIAN_POINT ( 'NONE',  ( -0.1993543840281266355, 5.193138888964753619, 0.1993543840281267465 ) ) ;
#6655 = CARTESIAN_POINT ( 'NONE',  ( -0.2947723466326633290, 0.5822653189610053071, -1.096280161095893435 ) ) ;
#6656 = CARTESIAN_POINT ( 'NONE',  ( 0.000000000000000000, 0.000000000000000000, -0.01143517789850382292 ) ) ;
#6657 = DIRECTION ( 'NONE',  ( 2.169098857401406875E-15, 0.9767851838303063250, 0.2142211582677929216 ) ) ;
#6658 = CARTESIAN_POINT ( 'NONE',  ( -0.3119999999999999996, 4.050777777777777366, 0.000000000000000000 ) ) ;
#6659 = CONICAL_SURFACE ( 'NONE', #1602, 0.3308333333333332571, 0.7853981633974427279 ) ;
#6660 = CARTESIAN_POINT ( 'NONE',  ( -0.3119999999999999996, 5.224388889040620931, 0.000000000000000000 ) ) ;
#6661 = EDGE_CURVE ( 'NONE', #6278, #9761, #7613, .T. ) ;
#6662 = CARTESIAN_POINT ( 'NONE',  ( 0.1149486178008431447, 4.984919243813402900, -0.2909162232891184252 ) ) ;
#6663 = CARTESIAN_POINT ( 'NONE',  ( 3.820898013339742174E-17, 5.384999999999999787, 0.3119999999999999996 ) ) ;
#6664 = CARTESIAN_POINT ( 'NONE',  ( 0.4223136544080928201, 0.2974429753103076668, 0.07050986311825918618 ) ) ;
#6665 = ORIENTED_EDGE ( 'NONE', *, *, #15590, .F. ) ;
#6666 = CARTESIAN_POINT ( 'NONE',  ( -0.1839906024682744501, 4.882774787087751811, -0.2519870536740796974 ) ) ;
#6667 = CARTESIAN_POINT ( 'NONE',  ( 0.1658549492420689775, 4.132149360891332890, 0.2644516142144350268 ) ) ;
#6668 = CARTESIAN_POINT ( 'NONE',  ( 0.3155070326520292290, 0.1306872919485615736, 0.09701388888889106443 ) ) ;
#6669 = CARTESIAN_POINT ( 'NONE',  ( -0.2923287055106771337, 0.3973214284738861291, -0.2123892367102620804 ) ) ;
#6670 = EDGE_CURVE ( 'NONE', #15989, #21365, #13245, .T. ) ;
#6671 = PLANE ( 'NONE',  #22017 ) ;
#6672 = EDGE_CURVE ( 'NONE', #13943, #7960, #293, .T. ) ;
#6673 = CARTESIAN_POINT ( 'NONE',  ( -0.2233192592356399997, 0.1830357141881718830, 0.3073725909049499494 ) ) ;
#6674 = CARTESIAN_POINT ( 'NONE',  ( 0.1167790944451423257, 0.6013888888130223265, -0.2819296736111110424 ) ) ;
#6675 = CARTESIAN_POINT ( 'NONE',  ( 0.000000000000000000, 0.2764156081756484196, 0.02583333333333468970 ) ) ;
#6676 = CARTESIAN_POINT ( 'NONE',  ( 0.1294417382415921358, -0.3125000000000002220, 0.4181944444444491982 ) ) ;
#6677 = CARTESIAN_POINT ( 'NONE',  ( -0.2819296736111110979, 5.088972222298087544, 0.000000000000000000 ) ) ;
#6678 = CARTESIAN_POINT ( 'NONE',  ( 0.2764156081756483641, 0.1144950937579610056, 0.3487500000000040012 ) ) ;
#6679 = ORIENTED_EDGE ( 'NONE', *, *, #22252, .T. ) ;
#6680 = FACE_OUTER_BOUND ( 'NONE', #11036, .T. ) ;
#6681 = DIRECTION ( 'NONE',  ( -1.177540334020096602E-17, 0.2588190451025213501, -0.9659258262890682012 ) ) ;
#6682 = CARTESIAN_POINT ( 'NONE',  ( 0.3860879860166684940, 4.111524471938507119, -2.831872695974971599 ) ) ;
#6683 = CARTESIAN_POINT ( 'NONE',  ( 0.1292346314604056745, 0.4173611111111108496, -0.3119999999999999996 ) ) ;
#6684 = CARTESIAN_POINT ( 'NONE',  ( 0.3119999999999999996, 4.970916666666665762, -0.1292346314604056745 ) ) ;
#6685 = CARTESIAN_POINT ( 'NONE',  ( -0.2819296736111110979, 4.297305555631420582, 0.000000000000000000 ) ) ;
#6686 = CARTESIAN_POINT ( 'NONE',  ( -0.2819296736111110424, 3.925777777853644235, 0.1167790944451424923 ) ) ;
#6687 = CARTESIAN_POINT ( 'NONE',  ( 9.101228903679513089E-16, 0.2392857142857141850, 0.4000000000000000222 ) ) ;
#6688 = CARTESIAN_POINT ( 'NONE',  ( -0.1904260988303179414, 0.4204977338396926889, 0.4343746145485231080 ) ) ;
#6689 = CARTESIAN_POINT ( 'NONE',  ( 0.3108838931427311825, 4.807001385996093390, 0.02636691118709539108 ) ) ;
#6690 = EDGE_LOOP ( 'NONE', ( #14400, #12884, #14374, #16085 ) ) ;
#6691 = CARTESIAN_POINT ( 'NONE',  ( 0.2819296736111110979, 4.491750000075865223, -3.452642723725051716E-17 ) ) ;
#6692 = CARTESIAN_POINT ( 'NONE',  ( 0.000000000000000000, 0.000000000000000000, 1.326383476483184332 ) ) ;
#6693 = CARTESIAN_POINT ( 'NONE',  ( -0.2427454876524849925, 4.508203593491248107, 0.1960069984806188936 ) ) ;
#6694 = DATE_TIME_ROLE ( 'classification_date' ) ;
#6695 = CARTESIAN_POINT ( 'NONE',  ( -0.4687500000000003331, -0.08694130287036218319, 0.07655038602225107403 ) ) ;
#6696 = CARTESIAN_POINT ( 'NONE',  ( 0.1954553509668047195, 0.1954553509668046085, 0.06750000000000172529 ) ) ;
#6697 = CARTESIAN_POINT ( 'NONE',  ( 0.1900105704308386045, 5.206640035683666845, 0.2082794372640154323 ) ) ;
#6698 = CARTESIAN_POINT ( 'NONE',  ( -0.2819296736111110979, 4.144527777853643791, 0.000000000000000000 ) ) ;
#6699 = DATE_AND_TIME ( #4630, #2212 ) ;
#6700 = CARTESIAN_POINT ( 'NONE',  ( -0.3117958023240662846, 4.835187445956109720, -0.01167036106402472885 ) ) ;
#6701 = CARTESIAN_POINT ( 'NONE',  ( -3.827021247335479543E-17, -0.3125000000000000000, 0.2966666666666700203 ) ) ;
#6702 = CARTESIAN_POINT ( 'NONE',  ( -3.385114897866767815E-17, -0.2764156081756484196, 0.1647222222222247123 ) ) ;
#6703 = CARTESIAN_POINT ( 'NONE',  ( -0.2923287055106771337, 0.04017857133102902684, -0.2123892367102620804 ) ) ;
#6704 = APPLICATION_CONTEXT ( 'configuration controlled 3d designs of mechanical parts and assemblies' ) ;
#6705 = CARTESIAN_POINT ( 'NONE',  ( 0.1167790944451423257, 0.6152777777019110550, -0.2819296736111110424 ) ) ;
#6706 = CARTESIAN_POINT ( 'NONE',  ( -0.2872991414527177878, 0.07488537861673925933, 0.4079643588709177537 ) ) ;
#6707 = CARTESIAN_POINT ( 'NONE',  ( -0.4802535689586319156, 0.2139885278467183738, 0.05346681960559353242 ) ) ;
#6708 = PLANE ( 'NONE',  #19110 ) ;
#6709 = CARTESIAN_POINT ( 'NONE',  ( -0.1144950937579609918, -0.2764156081756484196, -0.01236111111111004406 ) ) ;
#6710 = CARTESIAN_POINT ( 'NONE',  ( 0.2230971623002953874, -0.2230971623002954429, 0.4164583333333376491 ) ) ;
#6711 = ORIENTED_EDGE ( 'NONE', *, *, #17864, .F. ) ;
#6712 = CARTESIAN_POINT ( 'NONE',  ( 0.8119709581221709049, 2.291712385858714285, -1.528283969076322801 ) ) ;
#6713 = CARTESIAN_POINT ( 'NONE',  ( -0.0005457459119219430560, 3.766070220202782703, -0.3119995940632557252 ) ) ;
#6714 = CARTESIAN_POINT ( 'NONE',  ( -0.1294417382415922746, -0.3125000000000000000, 0.01541666666666776514 ) ) ;
#6715 = CARTESIAN_POINT ( 'NONE',  ( -0.1993543840281267465, 0.3479166665908000611, 0.1993543840281266633 ) ) ;
#6716 = CARTESIAN_POINT ( 'NONE',  ( 0.1993543840281267465, 4.165361111186976828, 0.1993543840281266633 ) ) ;
#6717 = CARTESIAN_POINT ( 'NONE',  ( -0.2233192592356399442, -0.03482142866897095651, -0.3073725909049500049 ) ) ;
#6718 = ORIENTED_EDGE ( 'NONE', *, *, #19005, .F. ) ;
#6719 = VECTOR ( 'NONE', #18266, 39.37007874015748143 ) ;
#6720 = CARTESIAN_POINT ( 'NONE',  ( -0.1167790944451423535, 4.710500000075865223, 0.2819296736111110424 ) ) ;
#6721 = CARTESIAN_POINT ( 'NONE',  ( 0.1620925312155838405, 5.138945716096764649, -0.2584997478798148340 ) ) ;
#6722 = ADVANCED_FACE ( 'NONE', ( #15179 ), #22615, .F. ) ;
#6723 = CARTESIAN_POINT ( 'NONE',  ( 0.1292346314604057300, 0.3895833331816003775, 0.3119999999999998885 ) ) ;
#6724 = ORIENTED_EDGE ( 'NONE', *, *, #21938, .F. ) ;
#6725 = CARTESIAN_POINT ( 'NONE',  ( 0.000000000000000000, 5.384999999999999787, 0.000000000000000000 ) ) ;
#6726 = EDGE_CURVE ( 'NONE', #1635, #9081, #17091, .T. ) ;
#6727 = CARTESIAN_POINT ( 'NONE',  ( -0.1993543840281266355, 5.082027777853643791, 0.1993543840281267465 ) ) ;
#6728 = CARTESIAN_POINT ( 'NONE',  ( 0.1466396438660773627, 4.206187273484634837, -0.2762320324114326819 ) ) ;
#6729 = APPROVAL ( #5885, 'UNSPECIFIED' ) ;
#6730 = EDGE_LOOP ( 'NONE', ( #19431, #13130, #18423, #21553 ) ) ;
#6731 = CARTESIAN_POINT ( 'NONE',  ( 0.1167790944451422702, 4.891055555631421470, -0.2819296736111110979 ) ) ;
#6732 = PERSON_AND_ORGANIZATION_ROLE ( 'creator' ) ;
#6733 = AXIS2_PLACEMENT_3D ( 'NONE', #3939, #18809, #2105 ) ;
#6734 = CARTESIAN_POINT ( 'NONE',  ( -0.2513697473550708938, 5.108907442184293934, -0.1815747212199412541 ) ) ;
#6735 = CARTESIAN_POINT ( 'NONE',  ( -0.2206173157302028787, 0.2124999998482670627, 0.2206173157302027954 ) ) ;
#6736 = ORIENTED_EDGE ( 'NONE', *, *, #4559, .T. ) ;
#6737 = CARTESIAN_POINT ( 'NONE',  ( 1.726321361862525858E-17, 0.3965277777019111105, -0.2819296736111110979 ) ) ;
#6738 = DIRECTION ( 'NONE',  ( -0.7071067811865484609, 0.000000000000000000, -0.7071067811865464625 ) ) ;
#6739 = CARTESIAN_POINT ( 'NONE',  ( 0.1618212287091538581, 4.094532934258117152, -0.2700669807813751433 ) ) ;
#6740 = CARTESIAN_POINT ( 'NONE',  ( -0.2233192592356399997, 0.2544642856167432243, 0.3073725909049499494 ) ) ;
#6741 = CARTESIAN_POINT ( 'NONE',  ( -0.07784249766847600727, 5.069340931627631441, 0.3027131100711323852 ) ) ;
#6742 = DIRECTION ( 'NONE',  ( 0.4985709748471344183, 0.07555085810113186529, 0.8635502596144365439 ) ) ;
#6743 = LINE ( 'NONE', #5150, #16263 ) ;
#6744 = CARTESIAN_POINT ( 'NONE',  ( -0.2819296736111110424, 4.814666666742533074, 0.1167790944451424923 ) ) ;
#6745 = ORIENTED_EDGE ( 'NONE', *, *, #9740, .T. ) ;
#6746 = CARTESIAN_POINT ( 'NONE',  ( 1.990730333795405205, 2.661358883302036293, -2.647236895612580021 ) ) ;
#6747 = CARTESIAN_POINT ( 'NONE',  ( -0.2819296736111110424, 3.793833333409199149, -0.1167790944451423119 ) ) ;
#6748 = CARTESIAN_POINT ( 'NONE',  ( -0.2714878203009086777, 0.04947802436987754071, -0.1267951674310540955 ) ) ;
#6749 = CARTESIAN_POINT ( 'NONE',  ( 0.3118802040654409802, 5.028715422347283415, 0.04186130555678244797 ) ) ;
#6750 = CARTESIAN_POINT ( 'NONE',  ( -5.731347020009612645E-17, 0.4486111111111107386, 0.3119999999999999996 ) ) ;
#6751 = CARTESIAN_POINT ( 'NONE',  ( -0.4749999999999999778, 3.575000000000000622, 0.09499999999999995948 ) ) ;
#6752 = CARTESIAN_POINT ( 'NONE',  ( 5.731347020009612645E-17, 4.404944444596177178, 0.3119999999999999996 ) ) ;
#6753 = AXIS2_PLACEMENT_3D ( 'NONE', #14134, #8037, #13903 ) ;
#6754 = CARTESIAN_POINT ( 'NONE',  ( -0.1167790944451423535, 4.654944444520310753, 0.2819296736111110979 ) ) ;
#6755 = ORIENTED_EDGE ( 'NONE', *, *, #6632, .T. ) ;
#6756 = CARTESIAN_POINT ( 'NONE',  ( 0.1993543840281267465, 4.095916666742532186, 0.1993543840281266633 ) ) ;
#6757 = EDGE_CURVE ( 'NONE', #19892, #14569, #22123, .T. ) ;
#6758 = ORIENTED_EDGE ( 'NONE', *, *, #23915, .T. ) ;
#6759 = ORIENTED_EDGE ( 'NONE', *, *, #13343, .T. ) ;
#6760 = PERSON_AND_ORGANIZATION_ROLE ( 'design_owner' ) ;
#6761 = DIRECTION ( 'NONE',  ( 0.000000000000000000, 0.9659258262890680902, 0.2588190451025214611 ) ) ;
#6762 = CARTESIAN_POINT ( 'NONE',  ( 0.3387631043874195225, 2.661358883302036293, -0.9952696662045950049 ) ) ;
#6763 = EDGE_LOOP ( 'NONE', ( #22419, #6648, #20269, #16159 ) ) ;
#6764 = CARTESIAN_POINT ( 'NONE',  ( 1.910449006669871087E-17, 0.3583333331816003775, -0.3119999999999999996 ) ) ;
#6765 = CARTESIAN_POINT ( 'NONE',  ( -0.3120492848101305006, 4.389992572532343651, -0.04054563350898530288 ) ) ;
#6766 = AXIS2_PLACEMENT_3D ( 'NONE', #21945, #14646, #14402 ) ;
#6767 = CARTESIAN_POINT ( 'NONE',  ( -0.4687499999999811817, -0.08977042653030931074, 0.4243505787549145536 ) ) ;
#6768 = CARTESIAN_POINT ( 'NONE',  ( 0.4453125000000000000, 0.000000000000000000, 0.4425000000000000044 ) ) ;
#6769 = ORIENTED_EDGE ( 'NONE', *, *, #10189, .T. ) ;
#6770 = ORIENTED_EDGE ( 'NONE', *, *, #12728, .F. ) ;
#6771 = CARTESIAN_POINT ( 'NONE',  ( -0.3125000000000000000, 1.913510623667739771E-17, 0.3452777777777818469 ) ) ;
#6772 = CARTESIAN_POINT ( 'NONE',  ( 0.1993543840281266910, 0.6118055554796889561, -0.1993543840281266910 ) ) ;
#6773 = CARTESIAN_POINT ( 'NONE',  ( -0.1144950937579609779, 0.2764156081756484196, 0.02236111111111246247 ) ) ;
#6774 = CARTESIAN_POINT ( 'NONE',  ( -0.2819296736111110424, 4.523000000075865223, 0.1167790944451424923 ) ) ;
#6775 = CARTESIAN_POINT ( 'NONE',  ( -0.05866837512862337067, 0.2818896272181906082, -0.07694038459218610626 ) ) ;
#6776 = EDGE_CURVE ( 'NONE', #8220, #15596, #23502, .T. ) ;
#6777 = CARTESIAN_POINT ( 'NONE',  ( -0.1018020887675157859, 0.1946365182022625206, -1.235038816363745129 ) ) ;
#6778 = CARTESIAN_POINT ( 'NONE',  ( 0.3125000000000002220, -0.1294417382415921358, -0.02624999999999922187 ) ) ;
#6779 = CYLINDRICAL_SURFACE ( 'NONE', #7298, 0.2109499999999996656 ) ;
#6780 = ADVANCED_FACE ( 'NONE', ( #15535 ), #23074, .T. ) ;
#6781 = CARTESIAN_POINT ( 'NONE',  ( -0.1292346314604057023, 3.950083333333332281, 0.3119999999999998885 ) ) ;
#6782 = ADVANCED_FACE ( 'NONE', ( #13720 ), #21140, .F. ) ;
#6783 = CARTESIAN_POINT ( 'NONE',  ( -0.3125000000000004996, 0.1294417382415917195, 0.1681944444444467279 ) ) ;
#6784 = CARTESIAN_POINT ( 'NONE',  ( 0.3108730060166250975, 4.973664493242656803, 0.02649485966508354287 ) ) ;
#6785 = ORIENTED_EDGE ( 'NONE', *, *, #9016, .T. ) ;
#6786 = CARTESIAN_POINT ( 'NONE',  ( 0.000000000000000000, 3.738758431839877614E-19, -0.1012499999999999928 ) ) ;
#6787 = ORIENTED_EDGE ( 'NONE', *, *, #4886, .T. ) ;
#6788 = CARTESIAN_POINT ( 'NONE',  ( 0.03482881598886129748, 5.199150166515222438, 0.2833619536528675931 ) ) ;
#6789 = VECTOR ( 'NONE', #11384, 39.37007874015748143 ) ;
#6790 = ADVANCED_FACE ( 'NONE', ( #4070 ), #4193, .F. ) ;
#6791 = CARTESIAN_POINT ( 'NONE',  ( 0.2209708691207961651, 0.2209708691207959985, 0.2133333333333364001 ) ) ;
#6792 = CARTESIAN_POINT ( 'NONE',  ( -0.3155070326520292845, 1.931923388228935888E-17, 0.01020833333333479032 ) ) ;
#6793 = CARTESIAN_POINT ( 'NONE',  ( -0.3613381517857143232, 0.4008928570453146878, -0.1174058825155741004 ) ) ;
#6794 = AXIS2_PLACEMENT_3D ( 'NONE', #5254, #3795, #130 ) ;
#6795 = DIRECTION ( 'NONE',  ( -0.000000000000000000, -0.000000000000000000, -1.000000000000000000 ) ) ;
#6796 = PRODUCT_DEFINITION_SHAPE ( 'NONE', 'NONE',  #6872 ) ;
#6797 =( BOUNDED_CURVE ( )  B_SPLINE_CURVE ( 2, ( #14847, #17677, #964, #6574, #21567, #14024, #8521, #15961, #4860, #12326, #19085, #16786, #16897, #9830, #432, #1902, #17017, #5915, #13144, #13262, #9584, #2270, #5681, #14959, #17264, #7865, #9343, #312, #13375, #20559, #20679, #7749, #9705, #2148, #15314, #15193, #22744, #3970, #20438, #15081, #7982, #13500, #20915, #7630, #20796, #18850, #4209, #7512, #2393, #22262, #11661, #11542, #11181, #22631, #18610, #189, #22502, #547, #67, #5799, #22378, #11419, #11297, #5558, #13023, #3734, #18729, #2025, #672, #22972, #6275, #10073, #17494, #13731, #4442, #9949, #8218, #23088, #21278, #12030, #6396, #13847, #19442, #13617, #15435, #22861, #6152, #21032, #4325, #11778, #20972, #8280, #19385, #15372, #23032, #731, #15730, #23144, #9765, #19142, #2450, #13679, #5970, #611, #8042, #18911, #7810, #9889, #17436, #4147, #17317, #6456, #13908, #15491, #6092, #17203, #22920, #22800, #9642, #2211, #4269 ),
 .UNSPECIFIED., .F., .F. ) 
 B_SPLINE_CURVE_WITH_KNOTS ( ( 3, 2, 2, 2, 2, 2, 2, 2, 2, 2, 2, 2, 2, 2, 2, 2, 2, 2, 2, 2, 2, 2, 2, 2, 2, 2, 2, 2, 2, 2, 2, 2, 2, 2, 2, 2, 2, 2, 2, 2, 2, 2, 2, 2, 2, 2, 2, 2, 2, 2, 2, 2, 2, 2, 2, 2, 2, 2, 2, 2, 3 ),
 ( 0.1552981728545431983, 0.1571428571428571397, 0.1714285714285714302, 0.1857142857142857206, 0.2000000000000000111, 0.2142857142857142738, 0.2285714285714285643, 0.2428571428571428548, 0.2571428571428571175, 0.2714285714285714080, 0.2857142857142856984, 0.2999999999999999889, 0.3142857142857142794, 0.3285714285714285698, 0.3428571428571428603, 0.3571428571428571508, 0.3714285714285714413, 0.3857142857142857872, 0.4000000000000000222, 0.4142857142857142572, 0.4285714285714284921, 0.4428571428571428381, 0.4571428571428570731, 0.4714285714285714191, 0.4857142857142856540, 0.5000000000000000000, 0.5142857142857143460, 0.5285714285714285809, 0.5428571428571428159, 0.5571428571428571619, 0.5714285714285713969, 0.5857142857142857428, 0.5999999999999999778, 0.6142857142857144348, 0.6285714285714285587, 0.6428571428571429047, 0.6571428571428571397, 0.6714285714285713746, 0.6857142857142857206, 0.6999999999999999556, 0.7142857142857143016, 0.7285714285714285365, 0.7428571428571428825, 0.7571428571428572285, 0.7714285714285714635, 0.7857142857142856984, 0.8000000000000000444, 0.8142857142857142794, 0.8285714285714286254, 0.8428571428571428603, 0.8571428571428570953, 0.8714285714285713302, 0.8857142857142855652, 0.9000000000000000222, 0.9142857142857142572, 0.9285714285714286031, 0.9428571428571428381, 0.9571428571428571841, 0.9714285714285714191, 0.9857142857142857650, 1.000000000000000000 ),
 .UNSPECIFIED. ) 
 CURVE ( )  GEOMETRIC_REPRESENTATION_ITEM ( )  RATIONAL_B_SPLINE_CURVE ( ( 0.9889922301674729521, 0.9936800307216023809, 1.000000000000000000, 0.9510565162951535312, 1.000000000000000000, 0.9510565162951535312, 1.000000000000000000, 0.9510565162951535312, 1.000000000000000000, 0.9510565162951535312, 1.000000000000000000, 0.9510565162951535312, 1.000000000000000000, 0.9510565162951535312, 1.000000000000000000, 0.9510565162951535312, 1.000000000000000000, 0.9510565162951535312, 1.000000000000000000, 0.9510565162951535312, 1.000000000000000000, 0.9510565162951535312, 1.000000000000000000, 0.9510565162951535312, 1.000000000000000000, 0.9510565162951535312, 1.000000000000000000, 0.9510565162951535312, 1.000000000000000000, 0.9510565162951535312, 1.000000000000000000, 0.9510565162951535312, 1.000000000000000000, 0.9510565162951535312, 1.000000000000000000, 0.9510565162951535312, 1.000000000000000000, 0.9510565162951535312, 1.000000000000000000, 0.9510565162951535312, 1.000000000000000000, 0.9510565162951535312, 1.000000000000000000, 0.9510565162951535312, 1.000000000000000000, 0.9510565162951535312, 1.000000000000000000, 0.9510565162951535312, 1.000000000000000000, 0.9510565162951535312, 1.000000000000000000, 0.9510565162951535312, 1.000000000000000000, 0.9510565162951535312, 1.000000000000000000, 0.9510565162951535312, 1.000000000000000000, 0.9510565162951535312, 1.000000000000000000, 0.9510565162951535312, 1.000000000000000000, 0.9510565162951535312, 1.000000000000000000, 0.9510565162951535312, 1.000000000000000000, 0.9510565162951535312, 1.000000000000000000, 0.9510565162951535312, 1.000000000000000000, 0.9510565162951535312, 1.000000000000000000, 0.9510565162951535312, 1.000000000000000000, 0.9510565162951535312, 1.000000000000000000, 0.9510565162951535312, 1.000000000000000000, 0.9510565162951535312, 1.000000000000000000, 0.9510565162951535312, 1.000000000000000000, 0.9510565162951535312, 1.000000000000000000, 0.9510565162951535312, 1.000000000000000000, 0.9510565162951535312, 1.000000000000000000, 0.9510565162951535312, 1.000000000000000000, 0.9510565162951535312, 1.000000000000000000, 0.9510565162951535312, 1.000000000000000000, 0.9510565162951535312, 1.000000000000000000, 0.9510565162951535312, 1.000000000000000000, 0.9510565162951535312, 1.000000000000000000, 0.9510565162951535312, 1.000000000000000000, 0.9510565162951535312, 1.000000000000000000, 0.9510565162951535312, 1.000000000000000000, 0.9510565162951535312, 1.000000000000000000, 0.9510565162951535312, 1.000000000000000000, 0.9510565162951535312, 1.000000000000000000, 0.9510565162951535312, 1.000000000000000000, 0.9510565162951535312, 1.000000000000000000, 0.9510565162951535312, 1.000000000000000000, 0.9510565162951535312, 1.000000000000000000, 0.9510565162951535312, 1.000000000000000000 ) ) 
 REPRESENTATION_ITEM ( '' )  );
#6798 = CARTESIAN_POINT ( 'NONE',  ( 0.1116596296178199027, 0.2651785713310289561, 0.3436530038418508792 ) ) ;
#6799 = CARTESIAN_POINT ( 'NONE',  ( 0.000000000000000000, 0.2764156081756484196, -0.08527777777777729995 ) ) ;
#6800 = DIRECTION ( 'NONE',  ( -0.000000000000000000, -1.000000000000000000, -0.000000000000000000 ) ) ;
#6801 = CARTESIAN_POINT ( 'NONE',  ( 0.1993543840281266633, 5.068138888964754507, -0.1993543840281266910 ) ) ;
#6802 = DIRECTION ( 'NONE',  ( 0.000000000000000000, 0.000000000000000000, 1.000000000000000000 ) ) ;
#6803 = ORIENTED_EDGE ( 'NONE', *, *, #13522, .F. ) ;
#6804 = CARTESIAN_POINT ( 'NONE',  ( -0.1876531964494600191, 4.605128802226668761, -0.2492760297041929085 ) ) ;
#6805 = CARTESIAN_POINT ( 'NONE',  ( -0.2854188144692234586, 4.283709271031463039, 0.1301228050348401111 ) ) ;
#6806 = DIRECTION ( 'NONE',  ( 0.000000000000000000, -0.000000000000000000, -1.000000000000000000 ) ) ;
#6807 = CARTESIAN_POINT ( 'NONE',  ( 1.910449006669871087E-17, 0.5319444444444439979, -0.3119999999999999996 ) ) ;
#6808 = CARTESIAN_POINT ( 'NONE',  ( -1.910449006669871087E-17, 4.759111111111110404, -0.3119999999999999996 ) ) ;
#6809 = CARTESIAN_POINT ( 'NONE',  ( 0.2819296736111111534, 4.266055555631421470, 0.1167790944451422563 ) ) ;
#6810 = CARTESIAN_POINT ( 'NONE',  ( 0.2819296736111110424, 3.786888888964754507, -0.1167790944451423396 ) ) ;
#6811 = CARTESIAN_POINT ( 'NONE',  ( 0.000000000000000000, -2.347681869555226049E-17, 0.3425000000000000266 ) ) ;
#6812 = CARTESIAN_POINT ( 'NONE',  ( -0.3119999999999999996, 3.880638888888887639, -0.1292346314604056468 ) ) ;
#6813 = LOCAL_TIME ( 21, 9, 13.00000000000000000, #10727 ) ;
#6814 = DIRECTION ( 'NONE',  ( 1.000000000000000000, -0.000000000000000000, 1.224646799147353207E-16 ) ) ;
#6815 = CARTESIAN_POINT ( 'NONE',  ( 0.1167790944451422702, 4.557722222298087544, -0.2819296736111110424 ) ) ;
#6816 = EDGE_CURVE ( 'NONE', #17359, #15714, #19429, .T. ) ;
#6817 = CARTESIAN_POINT ( 'NONE',  ( 0.2351701443102654221, -0.2046330205462786322, 0.4229527702155532198 ) ) ;
#6818 = CARTESIAN_POINT ( 'NONE',  ( 0.4645572405553155537, -0.2721000128023693954, 0.05892738626661211260 ) ) ;
#6819 = VECTOR ( 'NONE', #23393, 39.37007874015748854 ) ;
#6820 = DATE_TIME_ROLE ( 'creation_date' ) ;
#6821 = CYLINDRICAL_SURFACE ( 'NONE', #22445, 0.01874999999999997155 ) ;
#6822 = CARTESIAN_POINT ( 'NONE',  ( 0.000000000000000000, 0.2764156081756484196, 0.01888888888889020401 ) ) ;
#6823 = CARTESIAN_POINT ( 'NONE',  ( -0.1167790944451423119, 4.023000000075866112, -0.2819296736111110979 ) ) ;
#6824 = CARTESIAN_POINT ( 'NONE',  ( -0.1536748323684310469, 4.826214147890177664, -0.2744405328660507459 ) ) ;
#6825 = CARTESIAN_POINT ( 'NONE',  ( 0.1294417382415921358, -0.3125000000000002220, 0.3001388888888922857 ) ) ;
#6826 = CARTESIAN_POINT ( 'NONE',  ( 0.1954553509668046640, -0.1954553509668047195, 0.2827777777777811807 ) ) ;
#6827 = SECURITY_CLASSIFICATION ( '', '', #18854 ) ;
#6828 = CARTESIAN_POINT ( 'NONE',  ( -0.3613381517857143232, 0.04374999990245759252, -0.1174058825155741004 ) ) ;
#6829 = CARTESIAN_POINT ( 'NONE',  ( -5.178964085587577574E-17, 0.02152777770191114173, 0.2819296736111110979 ) ) ;
#6830 = CARTESIAN_POINT ( 'NONE',  ( -0.1294417382415922191, 0.3125000000000000000, -0.05402777777777686280 ) ) ;
#6831 = CARTESIAN_POINT ( 'NONE',  ( 0.7333413623369199330, 2.740000000000000213, -0.4233948329531084243 ) ) ;
#6832 = FACE_BOUND ( 'NONE', #7981, .T. ) ;
#6833 = CARTESIAN_POINT ( 'NONE',  ( 0.4700000000000000844, 2.740000000000000213, -0.05000000000000028727 ) ) ;
#6834 = CARTESIAN_POINT ( 'NONE',  ( 0.3155070326520292845, -5.795770164686806123E-17, 0.4234027777777820689 ) ) ;
#6835 = ORIENTED_EDGE ( 'NONE', *, *, #14108, .F. ) ;
#6836 = VERTEX_POINT ( 'NONE', #20899 ) ;
#6837 = DIRECTION ( 'NONE',  ( -0.000000000000000000, -1.000000000000000000, -0.000000000000000000 ) ) ;
#6838 = CARTESIAN_POINT ( 'NONE',  ( -0.2726209726102415964, 3.840039493605415633, 0.1571297853222173302 ) ) ;
#6839 = CARTESIAN_POINT ( 'NONE',  ( 0.2819296736111110424, 0.3652777777019111105, 0.1167790944451424923 ) ) ;
#6840 = CARTESIAN_POINT ( 'NONE',  ( -0.1993543840281266355, 3.873694444520310309, 0.1993543840281267465 ) ) ;
#6841 = CARTESIAN_POINT ( 'NONE',  ( -0.3613381517857143232, -0.02767857152611381474, -0.1174058825155741004 ) ) ;
#6842 = VECTOR ( 'NONE', #2160, 39.37007874015748143 ) ;
#6843 = ORIENTED_EDGE ( 'NONE', *, *, #22259, .F. ) ;
#6844 = CARTESIAN_POINT ( 'NONE',  ( 0.2819296736111110424, 4.675777777853643791, -0.1167790944451423396 ) ) ;
#6845 = CARTESIAN_POINT ( 'NONE',  ( 0.1783598947430071191, 5.123355972270982051, 0.2511911702540504665 ) ) ;
#6846 = DIRECTION ( 'NONE',  ( -0.7071067811865436870, -0.7071067811865514585, -0.000000000000000000 ) ) ;
#6847 = ORIENTED_EDGE ( 'NONE', *, *, #19239, .T. ) ;
#6848 = CARTESIAN_POINT ( 'NONE',  ( 0.000000000000000000, 5.501232050807569607, 0.000000000000000000 ) ) ;
#6849 = CARTESIAN_POINT ( 'NONE',  ( -0.1993543840281266910, 5.068138888964754507, -0.1993543840281266910 ) ) ;
#6850 = CC_DESIGN_SECURITY_CLASSIFICATION ( #3736, ( #24133 ) ) ;
#6851 = CARTESIAN_POINT ( 'NONE',  ( 0.2639807749865303310, 4.191608379692064013, 0.1663089970397409745 ) ) ;
#6852 =( NAMED_UNIT ( * ) PLANE_ANGLE_UNIT ( ) SI_UNIT ( $, .RADIAN. ) );
#6853 = VERTEX_POINT ( 'NONE', #2379 ) ;
#6854 = CARTESIAN_POINT ( 'NONE',  ( 5.178964085587577574E-17, 4.866750000075865223, 0.2819296736111110979 ) ) ;
#6855 = DATE_AND_TIME ( #18192, #23574 ) ;
#6856 = ORIENTED_EDGE ( 'NONE', *, *, #9327, .F. ) ;
#6857 = CARTESIAN_POINT ( 'NONE',  ( -1.903245722532910002E-17, 5.100068075568266579, -0.3108236144263021861 ) ) ;
#6858 = CARTESIAN_POINT ( 'NONE',  ( 0.1292346314604056745, 0.2506944444444441089, -0.3119999999999999996 ) ) ;
#6859 = VERTEX_POINT ( 'NONE', #9815 ) ;
#6860 = CARTESIAN_POINT ( 'NONE',  ( -5.178964085587577574E-17, 0.2576388888130222155, 0.2819296736111110979 ) ) ;
#6861 = CARTESIAN_POINT ( 'NONE',  ( 0.2819296736111110424, 0.05277777770191114520, -0.1167790944451423119 ) ) ;
#6862 = CARTESIAN_POINT ( 'NONE',  ( 0.4749999999999999778, 3.700000000000000622, -0.09499999999999995948 ) ) ;
#6863 = DIRECTION ( 'NONE',  ( -0.5000000000000012212, -0.8660254037844380415, 0.000000000000000000 ) ) ;
#6864 = CARTESIAN_POINT ( 'NONE',  ( -0.3236067977499790249, 0.08571428571428568732, 0.2351141009169892271 ) ) ;
#6865 = CARTESIAN_POINT ( 'NONE',  ( -0.09469529337756199538, 5.068847041801435083, 0.2977286714186166972 ) ) ;
#6866 = CARTESIAN_POINT ( 'NONE',  ( 0.2206173157302027954, 4.196611111111110404, -0.2206173157302028232 ) ) ;
#6867 = CYLINDRICAL_SURFACE ( 'NONE', #7689, 0.7500000000000001110 ) ;
#6868 = CARTESIAN_POINT ( 'NONE',  ( -0.2819296736111110979, 4.755638888964754507, 0.000000000000000000 ) ) ;
#6869 = EDGE_LOOP ( 'NONE', ( #1998, #3190, #12460, #3888 ) ) ;
#6870 = CARTESIAN_POINT ( 'NONE',  ( 0.2275323619091996763, 4.536638745974315157, -0.2154182091710123426 ) ) ;
#6871 = CARTESIAN_POINT ( 'NONE',  ( -0.2819296736111110979, 5.255638888964754507, 0.000000000000000000 ) ) ;
#6872 = PRODUCT_DEFINITION ( 'UNKNOWN', '', #8363, #6309 ) ;
#6873 = CARTESIAN_POINT ( 'NONE',  ( 0.4687500000000003886, 0.04389001238043919312, 0.09139217099949126233 ) ) ;
#6874 = CARTESIAN_POINT ( 'NONE',  ( 0.3125000000000000000, -5.740531871003217465E-17, -0.07138888888888809958 ) ) ;
#6875 = CARTESIAN_POINT ( 'NONE',  ( -0.4678785457174671758, -0.2663437566607215756, 0.05892894635879406678 ) ) ;
#6876 = VECTOR ( 'NONE', #15619, 39.37007874015748143 ) ;
#6877 = CARTESIAN_POINT ( 'NONE',  ( -0.04622087296078272040, 4.792553729289763531, 0.3085726088726347127 ) ) ;
#6878 = CARTESIAN_POINT ( 'NONE',  ( -0.2206173157302027676, 4.231333333485065573, 0.2206173157302028787 ) ) ;
#6879 = B_SPLINE_CURVE_WITH_KNOTS ( 'NONE', 3,
 ( #4138, #13426, #2206, #17067, #13672, #361, #2321, #22911, #4376, #9757, #22793, #6208, #4262, #15245, #481, #17430, #21086, #15485 ),
 .UNSPECIFIED., .F., .F.,
 ( 4, 2, 2, 2, 2, 2, 2, 2, 4 ),
 ( 0.5756575327745111492, 0.5779426686689235204, 0.5802278045633358916, 0.5825129404577482628, 0.5847980763521607450, 0.5870832122465731162, 0.5893683481409854874, 0.5916534840353978586, 0.5939386199298102298 ),
 .UNSPECIFIED. ) ;
#6880 = CARTESIAN_POINT ( 'NONE',  ( 0.2819296736111110979, 4.786888888964754507, -0.1167790944451423396 ) ) ;
#6881 = EDGE_LOOP ( 'NONE', ( #4210, #678, #16413, #459 ) ) ;
#6882 = CARTESIAN_POINT ( 'NONE',  ( 0.2819296736111110424, 3.884111111186976384, -0.1167790944451423396 ) ) ;
#6883 = VERTEX_POINT ( 'NONE', #21857 ) ;
#6884 = PERSON_AND_ORGANIZATION ( #15518, #2538 ) ;
#6885 = DIRECTION ( 'NONE',  ( -0.000000000000000000, -1.000000000000000000, -0.000000000000000000 ) ) ;
#6886 = CARTESIAN_POINT ( 'NONE',  ( -0.1294417382415922746, -0.3125000000000000000, 0.2445833333333366777 ) ) ;
#6887 = ADVANCED_FACE ( 'NONE', ( #17968 ), #8934, .T. ) ;
#6888 = ORIENTED_EDGE ( 'NONE', *, *, #1111, .F. ) ;
#6889 = CARTESIAN_POINT ( 'NONE',  ( 0.3119999999999998885, 0.2854166665149337478, 0.1292346314604058410 ) ) ;
#6890 = CARTESIAN_POINT ( 'NONE',  ( 0.3146687483788559447, 0.3722097299877928367, 0.07156199457778794626 ) ) ;
#6891 = CIRCLE ( 'NONE', #15834, 0.3150000000000000022 ) ;
#6892 = CARTESIAN_POINT ( 'NONE',  ( -0.2015352175386056210, 4.383312114150648142, -0.2394718385862008581 ) ) ;
#6893 = EDGE_CURVE ( 'NONE', #17266, #19560, #3744, .T. ) ;
#6894 = CARTESIAN_POINT ( 'NONE',  ( 0.3125000000000000000, -5.740531871003217465E-17, -0.07833333333333296344 ) ) ;
#6895 = CARTESIAN_POINT ( 'NONE',  ( 0.000000000000000000, 5.384999999999999787, -0.3119999999999999996 ) ) ;
#6896 = B_SPLINE_CURVE_WITH_KNOTS ( 'NONE', 3,
 ( #15489, #22917, #6212, #13677, #123, #2078, #249, #7684 ),
 .UNSPECIFIED., .F., .F.,
 ( 4, 2, 2, 4 ),
 ( 0.000000000000000000, 0.0004997454757086376362, 0.0007496182135629577553, 0.0009994909514172778744 ),
 .UNSPECIFIED. ) ;
#6897 = EDGE_LOOP ( 'NONE', ( #21623, #11677, #22304, #23414, #11938, #10743, #2395, #14729, #6603, #11908, #1591, #6908, #12249, #4423, #20661, #18370, #3856, #19805, #17653, #4541, #8708, #17477, #8789, #3611, #23879, #15109, #13632, #6153, #13886, #6393, #21152, #15059, #9121, #5659, #8754, #18354, #5424, #23530, #1302, #9, #17553, #5178, #3803, #6017, #10567, #23463, #2406, #19246, #8219, #12207, #20850, #12632, #2510, #11648, #12144, #13430, #6137 ) ) ;
#6898 = CARTESIAN_POINT ( 'NONE',  ( 0.4700000000000001954, 2.740000000000000213, 0.000000000000000000 ) ) ;
#6899 = CARTESIAN_POINT ( 'NONE',  ( -0.1993543840281266633, 0.3340277777019111660, -0.1993543840281266910 ) ) ;
#6900 = CARTESIAN_POINT ( 'NONE',  ( 0.1954553509668046640, -0.1954553509668047195, 0.1647222222222247123 ) ) ;
#6901 = EDGE_CURVE ( 'NONE', #3858, #7205, #4786, .T. ) ;
#6902 = CARTESIAN_POINT ( 'NONE',  ( 0.2819296736111110979, 4.380638888964754507, -3.452642723725051716E-17 ) ) ;
#6903 = CARTESIAN_POINT ( 'NONE',  ( 0.04489076912979098055, 0.2868701433674690215, -0.07891441836899415474 ) ) ;
#6904 = DIRECTION ( 'NONE',  ( -0.000000000000000000, -1.000000000000000000, -0.000000000000000000 ) ) ;
#6905 = CARTESIAN_POINT ( 'NONE',  ( 0.000000000000000000, 5.501232050807569607, 0.000000000000000000 ) ) ;
#6906 = CARTESIAN_POINT ( 'NONE',  ( -0.3119999999999999996, 3.991749999999999243, -0.1292346314604056468 ) ) ;
#6907 = CARTESIAN_POINT ( 'NONE',  ( 0.3119999999999999996, 4.866750000151731648, -0.1292346314604056745 ) ) ;
#6908 = ORIENTED_EDGE ( 'NONE', *, *, #12477, .T. ) ;
#6909 = CIRCLE ( 'NONE', #4949, 0.01875000000000000971 ) ;
#6910 = CARTESIAN_POINT ( 'NONE',  ( -0.3125000000000000000, 1.913510623667739771E-17, -0.09916666666666609786 ) ) ;
#6911 = ORIENTED_EDGE ( 'NONE', *, *, #9494, .F. ) ;
#6912 = DIRECTION ( 'NONE',  ( 0.8660254037844383745, 0.000000000000000000, 0.5000000000000004441 ) ) ;
#6913 = EDGE_CURVE ( 'NONE', #12181, #5059, #19881, .T. ) ;
#6914 = CARTESIAN_POINT ( 'NONE',  ( 0.3155070326520292290, -0.1306872919485616569, 0.3122916666666705754 ) ) ;
#6915 = CARTESIAN_POINT ( 'NONE',  ( 0.3613381517857143232, 0.3651785713310288783, 0.1174058825155742114 ) ) ;
#6916 = EDGE_CURVE ( 'NONE', #22476, #13713, #13592, .T. ) ;
#6917 = ORIENTED_EDGE ( 'NONE', *, *, #2055, .F. ) ;
#6918 = CARTESIAN_POINT ( 'NONE',  ( -0.3119999999999998885, 4.443138888888888083, 0.1292346314604058410 ) ) ;
#6919 = CARTESIAN_POINT ( 'NONE',  ( -0.1116596296178200276, 0.1866071427596004417, 0.3436530038418508792 ) ) ;
#6920 = CIRCLE ( 'NONE', #21725, 0.3385998376278290256 ) ;
#6921 = CARTESIAN_POINT ( 'NONE',  ( 0.2819296736111110424, 0.1569444443685777679, 0.1167790944451424923 ) ) ;
#6922 = CARTESIAN_POINT ( 'NONE',  ( -3.385114897866767815E-17, -0.2764156081756484196, -0.001944444444443294917 ) ) ;
#6923 = CARTESIAN_POINT ( 'NONE',  ( -0.2819296736111110979, 5.255638888964754507, 0.000000000000000000 ) ) ;
#6924 = CARTESIAN_POINT ( 'NONE',  ( 0.06854178015534857782, 4.486376190189668378, -0.3045296682676547073 ) ) ;
#6925 = EDGE_CURVE ( 'NONE', #20833, #7372, #20393, .T. ) ;
#6926 = VERTEX_POINT ( 'NONE', #1619 ) ;
#6927 = FACE_OUTER_BOUND ( 'NONE', #5321, .T. ) ;
#6928 = DIRECTION ( 'NONE',  ( 0.000000000000000000, 0.9659258262890682012, 0.2588190451025213501 ) ) ;
#6929 = CARTESIAN_POINT ( 'NONE',  ( -0.4592340600545777307, -0.08946199657451012199, 0.4305916167228413527 ) ) ;
#6930 = CARTESIAN_POINT ( 'NONE',  ( 0.2782497666485165277, 0.06249891821425377497, 0.1411420113220940853 ) ) ;
#6931 = CARTESIAN_POINT ( 'NONE',  ( 0.3119999999999999996, 4.797305555555554157, 0.1292346314604056190 ) ) ;
#6932 = CARTESIAN_POINT ( 'NONE',  ( 0.1167790944451424506, 3.925777777853643347, 0.2819296736111110424 ) ) ;
#6933 = CARTESIAN_POINT ( 'NONE',  ( 0.1797087373818229139, 3.735609845915246474, -0.2172305470487487511 ) ) ;
#6934 = DIRECTION ( 'NONE',  ( 0.000000000000000000, -1.000000000000000000, 0.000000000000000000 ) ) ;
#6935 = CARTESIAN_POINT ( 'NONE',  ( 0.2206173157302027954, 4.418833333333332725, -0.2206173157302028232 ) ) ;
#6936 = ORIENTED_EDGE ( 'NONE', *, *, #6029, .F. ) ;
#6937 = CARTESIAN_POINT ( 'NONE',  ( -0.2206173157302027676, 4.557722222222221120, 0.2206173157302028787 ) ) ;
#6938 = CARTESIAN_POINT ( 'NONE',  ( 0.1993543840281266633, 4.498694444520309865, -0.1993543840281266910 ) ) ;
#6939 = B_SPLINE_CURVE_WITH_KNOTS ( 'NONE', 3,
 ( #16437, #14740, #12920, #16676, #7409, #23725, #20091, #23847, #5572, #5452, #9107, #9359, #7050, #6924, #20453, #14860, #22034, #21792, #3749, #8871, #5081, #3256, #11193, #14362, #5330, #11070, #10833, #20331, #7167, #12549, #16556, #23978, #7289, #19969, #18142, #21911, #5200, #22155, #20934, #11435, #5812, #13391, #20813, #82, #20574, #7767, #6051 ),
 .UNSPECIFIED., .F., .F.,
 ( 4, 2, 1, 2, 2, 1, 1, 2, 2, 2, 2, 2, 2, 2, 2, 2, 1, 1, 2, 2, 1, 1, 2, 2, 2, 2, 4 ),
 ( 0.4842883486437473683, 0.4848597289547300071, 0.4851454191102213542, 0.4852882641879670556, 0.4853061198226852335, 0.4853239754574034670, 0.4853596867268398785, 0.4854311092657127014, 0.4865738698876779234, 0.4877166305096431453, 0.4888593911316083673, 0.4900021517535736448, 0.4911449123755388668, 0.4922876729975040888, 0.4934304336194693108, 0.4945731942414345328, 0.4946446167803074112, 0.4946624724150255892, 0.4946714002323847059, 0.4946803280497438227, 0.4947160393191802341, 0.4948588843969258799, 0.4951445745524171160, 0.4957159548633996993, 0.4980014761073300322, 0.5002869973512602542, 0.5025725185951905871 ),
 .UNSPECIFIED. ) ;
#6940 = CARTESIAN_POINT ( 'NONE',  ( -0.2806174154849702118, 4.506217266555575307, 0.1379780153053364600 ) ) ;
#6941 = VECTOR ( 'NONE', #4090, 39.37007874015748143 ) ;
#6942 = PERSON_AND_ORGANIZATION ( #15518, #2538 ) ;
#6943 = CARTESIAN_POINT ( 'NONE',  ( -1.296004783052830448E-07, 4.710500003633881327, -0.3119999999999730766 ) ) ;
#6944 =( BOUNDED_CURVE ( )  B_SPLINE_CURVE ( 2, ( #18506, #19975, #23730, #22041, #5336, #18267, #8999, #20098, #7055 ),
 .UNSPECIFIED., .F., .F. ) 
 B_SPLINE_CURVE_WITH_KNOTS ( ( 3, 2, 2, 2, 3 ),
 ( 0.8125000000000000000, 0.8229166666666666297, 0.8333333333333333703, 0.8437500000000000000, 0.8541666666666666297 ),
 .UNSPECIFIED. ) 
 CURVE ( )  GEOMETRIC_REPRESENTATION_ITEM ( )  RATIONAL_B_SPLINE_CURVE ( ( 1.000000000000000000, 0.9238795325112867385, 1.000000000000000000, 0.9238795325112867385, 1.000000000000000000, 0.9238795325112867385, 1.000000000000000000, 0.9238795325112867385, 1.000000000000000000 ) ) 
 REPRESENTATION_ITEM ( '' )  );
#6945 = ADVANCED_FACE ( 'NONE', ( #18321 ), #22332, .T. ) ;
#6946 = CARTESIAN_POINT ( 'NONE',  ( 0.2764156081756483641, 0.1144950937579610056, -0.04708333333333254017 ) ) ;
#6947 = ADVANCED_FACE ( 'NONE', ( #20153 ), #8840, .F. ) ;
#6948 = CARTESIAN_POINT ( 'NONE',  ( -1.726321361862525858E-17, 4.075083333409199149, -0.2819296736111110979 ) ) ;
#6949 = CARTESIAN_POINT ( 'NONE',  ( -0.3079124582538622645, 4.834082022064681183, -0.05131535407519589864 ) ) ;
#6950 = CARTESIAN_POINT ( 'NONE',  ( -0.2209708691207961373, -0.2209708691207961095, 0.2897222222222255450 ) ) ;
#6951 = CARTESIAN_POINT ( 'NONE',  ( -0.1954553509668046918, -0.1954553509668046640, 0.3244444444444481435 ) ) ;
#6952 = CARTESIAN_POINT ( 'NONE',  ( -0.3613381517857144343, 0.05089285704531474469, 0.1174058825155740171 ) ) ;
#6953 = CARTESIAN_POINT ( 'NONE',  ( -0.1993543840281266633, 0.0006944443685778107491, -0.1993543840281266910 ) ) ;
#6954 = CARTESIAN_POINT ( 'NONE',  ( 0.03071979988720062796, 0.2873147545066538355, 0.3999952370221915854 ) ) ;
#6955 = CARTESIAN_POINT ( 'NONE',  ( -0.1854441301479783366, 0.2626830736182380610, -0.7267533148750512373 ) ) ;
#6956 = CARTESIAN_POINT ( 'NONE',  ( 0.2764156081756483641, -0.1144950937579611028, -0.05402777777777704321 ) ) ;
#6957 = CARTESIAN_POINT ( 'NONE',  ( -0.1306872919485614903, 0.3155070326520293400, 0.3852083333333373161 ) ) ;
#6958 = EDGE_CURVE ( 'NONE', #17046, #18346, #1907, .T. ) ;
#6959 = VERTEX_POINT ( 'NONE', #21678 ) ;
#6960 = ORIENTED_EDGE ( 'NONE', *, *, #22035, .F. ) ;
#6961 = CARTESIAN_POINT ( 'NONE',  ( -0.4000000000000000222, 0.07857142857142855596, -4.898587196589413075E-17 ) ) ;
#6962 = DIRECTION ( 'NONE',  ( 0.3273051541876792481, 0.6681584153635196088, -0.6681584153635196088 ) ) ;
#6963 = CARTESIAN_POINT ( 'NONE',  ( -5.178964085587577574E-17, 0.5215277777019111660, 0.2819296736111110979 ) ) ;
#6964 = CARTESIAN_POINT ( 'NONE',  ( 0.2819296736111110979, 3.783416666742532186, -3.452642723725051716E-17 ) ) ;
#6965 = AXIS2_PLACEMENT_3D ( 'NONE', #17272, #4335, #13741 ) ;
#6966 = CARTESIAN_POINT ( 'NONE',  ( 0.2923287055106771337, 0.07589285704531474608, 0.2123892367102621359 ) ) ;
#6967 = CARTESIAN_POINT ( 'NONE',  ( -1.726321361862525858E-17, 4.463972222298087544, -0.2819296736111110979 ) ) ;
#6968 = CARTESIAN_POINT ( 'NONE',  ( 0.03989520295803244965, 5.142369579426448567, -0.3022423214455481899 ) ) ;
#6969 = DIRECTION ( 'NONE',  ( 0.000000000000000000, 0.000000000000000000, 1.000000000000000000 ) ) ;
#6970 = EDGE_LOOP ( 'NONE', ( #15027, #23786, #11270, #7447 ) ) ;
#6971 = CARTESIAN_POINT ( 'NONE',  ( 0.3021975922303085649, 4.365644181327585471, -0.08256521648007630887 ) ) ;
#6972 = CARTESIAN_POINT ( 'NONE',  ( -0.2819296736111110424, 5.127166666742532186, -0.1167790944451423119 ) ) ;
#6973 = FACE_OUTER_BOUND ( 'NONE', #18495, .T. ) ;
#6974 = CARTESIAN_POINT ( 'NONE',  ( 0.000000000000000000, 3.659999999999999698, -0.3125000000000000000 ) ) ;
#6975 = AXIS2_PLACEMENT_3D ( 'NONE', #1548, #5072, #4955 ) ;
#6976 = CARTESIAN_POINT ( 'NONE',  ( 0.1167790944451422702, 4.835500000075865223, -0.2819296736111110979 ) ) ;
#6977 = APPROVAL_ROLE ( '' ) ;
#6978 = VERTEX_POINT ( 'NONE', #13771 ) ;
#6979 = DIRECTION ( 'NONE',  ( -0.000000000000000000, -1.000000000000000000, 0.000000000000000000 ) ) ;
#6980 = CARTESIAN_POINT ( 'NONE',  ( -0.03984146987716615657, 4.544964378884258416, -0.3119997632626998474 ) ) ;
#6981 = ORIENTED_EDGE ( 'NONE', *, *, #13947, .T. ) ;
#6982 = CARTESIAN_POINT ( 'NONE',  ( -0.1993543840281267465, 0.3618055554796889006, 0.1993543840281266633 ) ) ;
#6983 = EDGE_LOOP ( 'NONE', ( #11840, #13353, #5042, #2297 ) ) ;
#6984 = CARTESIAN_POINT ( 'NONE',  ( -0.1993543840281267465, 0.08402777770191115214, 0.1993543840281266633 ) ) ;
#6985 = EDGE_CURVE ( 'NONE', #22531, #4780, #2319, .T. ) ;
#6986 = DIRECTION ( 'NONE',  ( 6.123233995736811642E-17, 0.000000000000000000, -1.000000000000000000 ) ) ;
#6987 = CARTESIAN_POINT ( 'NONE',  ( -0.5116234456863466562, 3.685658299244018554, 2.549370209580444691 ) ) ;
#6988 = CARTESIAN_POINT ( 'NONE',  ( 0.3236067977499789694, -0.03571428571428573312, 0.2351141009169893659 ) ) ;
#6989 = CARTESIAN_POINT ( 'NONE',  ( -0.09802781027409257497, 5.046564986788329321, -0.2971681987422591931 ) ) ;
#6990 = DIRECTION ( 'NONE',  ( -1.224646799147353207E-16, 1.000000000000000000, 0.000000000000000000 ) ) ;
#6991 = CARTESIAN_POINT ( 'NONE',  ( -0.3125000000000000000, 1.913510623667739771E-17, 0.06750000000000189182 ) ) ;
#6992 = DIRECTION ( 'NONE',  ( 0.000000000000000000, 0.000000000000000000, -1.000000000000000000 ) ) ;
#6993 = CARTESIAN_POINT ( 'NONE',  ( 0.1993543840281267465, 4.443138888964754507, 0.1993543840281266633 ) ) ;
#6994 = DIRECTION ( 'NONE',  ( 0.000000000000000000, -0.000000000000000000, 1.000000000000000000 ) ) ;
#6995 = CARTESIAN_POINT ( 'NONE',  ( 0.2251296462303276347, 4.523151383338628762, 0.2168217435695329043 ) ) ;
#6996 = CARTESIAN_POINT ( 'NONE',  ( 0.2819296736111110979, 5.057722222298088433, 0.1167790944451422425 ) ) ;
#6997 = CARTESIAN_POINT ( 'NONE',  ( 1.791833110003796271E-17, 0.04312855400452411669, -0.2926285540045244216 ) ) ;
#6998 = CARTESIAN_POINT ( 'NONE',  ( 0.2674007968890174669, 3.757045421648967487, -0.1629501482939255674 ) ) ;
#6999 = CARTESIAN_POINT ( 'NONE',  ( -0.4683334081279688643, -0.2655573993979173375, 0.04698409998688869021 ) ) ;
#7000 = VECTOR ( 'NONE', #22409, 39.37007874015748143 ) ;
#7001 = ORIENTED_EDGE ( 'NONE', *, *, #22714, .T. ) ;
#7002 = CARTESIAN_POINT ( 'NONE',  ( -0.1019843081256275041, 4.790927999518966196, 0.2955334162662792141 ) ) ;
#7003 = CARTESIAN_POINT ( 'NONE',  ( 0.1292346314604058410, 4.297305555707287894, 0.3119999999999998885 ) ) ;
#7004 = CARTESIAN_POINT ( 'NONE',  ( 0.1993543840281266633, 4.734805555631421470, -0.1993543840281266910 ) ) ;
#7005 = CARTESIAN_POINT ( 'NONE',  ( -1.726321361862525858E-17, 3.950083333409199149, -0.2819296736111110979 ) ) ;
#7006 = PRODUCT ( 'Aloris-BXA-Handle-Rod', 'Aloris-BXA-Handle-Rod', '', ( #21995 ) ) ;
#7007 = ORIENTED_EDGE ( 'NONE', *, *, #7681, .F. ) ;
#7008 = ORIENTED_EDGE ( 'NONE', *, *, #12445, .T. ) ;
#7009 = PERSON_AND_ORGANIZATION_ROLE ( 'design_owner' ) ;
#7010 = CC_DESIGN_DATE_AND_TIME_ASSIGNMENT ( #19684, #17865, ( #19252 ) ) ;
#7011 = AXIS2_PLACEMENT_3D ( 'NONE', #16525, #16646, #46 ) ;
#7012 = CARTESIAN_POINT ( 'NONE',  ( 0.1514837979169836590, -0.4428147562410877369, 0.4304954382810344260 ) ) ;
#7013 = DIRECTION ( 'NONE',  ( 0.000000000000000000, -1.000000000000000000, 0.000000000000000000 ) ) ;
#7014 = ORIENTED_EDGE ( 'NONE', *, *, #3237, .T. ) ;
#7015 = CARTESIAN_POINT ( 'NONE',  ( -5.731347020009612645E-17, 0.3305555554038226429, 0.3119999999999999996 ) ) ;
#7016 = AXIS2_PLACEMENT_3D ( 'NONE', #5149, #14915, #3204 ) ;
#7017 = CARTESIAN_POINT ( 'NONE',  ( 1.364852645245658621E-07, 4.377166663151471404, -0.3119999999999701346 ) ) ;
#7018 = DIRECTION ( 'NONE',  ( 0.000000000000000000, 0.000000000000000000, -1.000000000000000000 ) ) ;
#7019 = CARTESIAN_POINT ( 'NONE',  ( 0.000000000000000000, 3.738758431839877614E-19, -0.1199999999999999956 ) ) ;
#7020 = DIRECTION ( 'NONE',  ( -0.000000000000000000, -1.000000000000000000, -0.000000000000000000 ) ) ;
#7021 = ORIENTED_EDGE ( 'NONE', *, *, #12849, .T. ) ;
#7022 = DIRECTION ( 'NONE',  ( -0.000000000000000000, -0.9961946980917454342, 0.08715574274765830465 ) ) ;
#7023 = CARTESIAN_POINT ( 'NONE',  ( 1.726321361862525858E-17, 0.1604166665908000333, -0.2819296736111110979 ) ) ;
#7024 = CARTESIAN_POINT ( 'NONE',  ( -0.2764156081756484196, 0.1144950937579609918, 0.3626388888888929518 ) ) ;
#7025 = VERTEX_POINT ( 'NONE', #11955 ) ;
#7026 = CARTESIAN_POINT ( 'NONE',  ( 0.2819296736111110979, 4.432722222298088433, 0.1167790944451422425 ) ) ;
#7027 = CARTESIAN_POINT ( 'NONE',  ( 1.910449006669871087E-17, 0.1986111111111107386, -0.3119999999999999996 ) ) ;
#7028 = CARTESIAN_POINT ( 'NONE',  ( -0.03677510111069775406, -0.5081344126854103749, 0.4062297518000713703 ) ) ;
#7029 = PLANE ( 'NONE',  #12011 ) ;
#7030 = ADVANCED_FACE ( 'NONE', ( #6438 ), #13892, .T. ) ;
#7031 = CARTESIAN_POINT ( 'NONE',  ( 0.3119999999999999996, 4.022999999999998799, -3.820898013339742174E-17 ) ) ;
#7032 = CARTESIAN_POINT ( 'NONE',  ( 0.1292346314604056190, 4.984805555707287006, -0.3119999999999999996 ) ) ;
#7033 = AXIS2_PLACEMENT_3D ( 'NONE', #21440, #6681, #6928 ) ;
#7034 = AXIS2_PLACEMENT_3D ( 'NONE', #425, #21389, #9943 ) ;
#7035 = CARTESIAN_POINT ( 'NONE',  ( 0.3120000000000000551, 4.852861111111110404, 0.1292346314604056190 ) ) ;
#7036 = EDGE_CURVE ( 'NONE', #23454, #7806, #13977, .T. ) ;
#7037 = CARTESIAN_POINT ( 'NONE',  ( -8.252060436089559755E-07, 4.682689096385127314, 0.3119999999976427185 ) ) ;
#7038 = CC_DESIGN_DATE_AND_TIME_ASSIGNMENT ( #10256, #15499, ( #15437 ) ) ;
#7039 = EDGE_CURVE ( 'NONE', #6611, #14348, #18622, .T. ) ;
#7040 = CARTESIAN_POINT ( 'NONE',  ( -0.3155070326520293400, -0.1306872919485614626, 0.1803472222222250454 ) ) ;
#7041 = CARTESIAN_POINT ( 'NONE',  ( -0.2923287055106771337, 0.3401785713310290227, 0.2123892367102619971 ) ) ;
#7042 = ORIENTED_EDGE ( 'NONE', *, *, #13328, .F. ) ;
#7043 = CARTESIAN_POINT ( 'NONE',  ( 0.3236067977499790249, 0.04999999999999996114, -0.2351141009169892826 ) ) ;
#7044 = VECTOR ( 'NONE', #2367, 39.37007874015748143 ) ;
#7045 = CARTESIAN_POINT ( 'NONE',  ( -0.3613381517857143232, 0.1723214284738861513, -4.425116109941954795E-17 ) ) ;
#7046 = AXIS2_PLACEMENT_3D ( 'NONE', #376, #4155, #19510 ) ;
#7047 = CARTESIAN_POINT ( 'NONE',  ( 1.726321361862525858E-17, 0.2854166665908000056, -0.2819296736111110979 ) ) ;
#7048 = CARTESIAN_POINT ( 'NONE',  ( 0.000000000000000000, 0.2764156081756484196, 0.1925000000000026690 ) ) ;
#7049 = CARTESIAN_POINT ( 'NONE',  ( -0.2819296736111110424, 5.085500000075866112, -0.1167790944451423119 ) ) ;
#7050 = CARTESIAN_POINT ( 'NONE',  ( 0.06089257667514946099, 4.486588928204580107, -0.3060585940131039240 ) ) ;
#7051 = VERTEX_POINT ( 'NONE', #18499 ) ;
#7052 = CYLINDRICAL_SURFACE ( 'NONE', #9521, 0.3119999999999999996 ) ;
#7053 = CARTESIAN_POINT ( 'NONE',  ( 0.003006042110193701388, 4.877085829448629895, -0.3119876125383257426 ) ) ;
#7054 = CARTESIAN_POINT ( 'NONE',  ( 1.573500000000000343, 0.5250000000000000222, -0.5399999999999998135 ) ) ;
#7055 = CARTESIAN_POINT ( 'NONE',  ( 1.910449006669871087E-17, 0.5805555554038225319, -0.3119999999999999996 ) ) ;
#7056 = CARTESIAN_POINT ( 'NONE',  ( 0.2206173157302027954, 4.807722222222221120, -0.2206173157302028232 ) ) ;
#7057 = CARTESIAN_POINT ( 'NONE',  ( 0.2819296736111110979, 3.995222222298087544, -0.1167790944451423396 ) ) ;
#7058 = CARTESIAN_POINT ( 'NONE',  ( 0.1167790944451424368, 3.828555555631421470, 0.2819296736111110424 ) ) ;
#7059 = CARTESIAN_POINT ( 'NONE',  ( 0.1744173410699168814, 4.038682005623637217, -0.2596828359170899048 ) ) ;
#7060 = CARTESIAN_POINT ( 'NONE',  ( 0.006464354918053449514, 0.5491938321437414006, 0.04193567535760748394 ) ) ;
#7061 = EDGE_LOOP ( 'NONE', ( #22630, #202, #12960, #11826 ) ) ;
#7062 = CARTESIAN_POINT ( 'NONE',  ( -0.3125000000000000000, 1.913510623667739771E-17, 0.1161111111111130384 ) ) ;
#7063 = EDGE_CURVE ( 'NONE', #7566, #5247, #1556, .T. ) ;
#7064 = CARTESIAN_POINT ( 'NONE',  ( 5.178964085587577574E-17, 4.533416666742532186, 0.2819296736111110979 ) ) ;
#7065 = CARTESIAN_POINT ( 'NONE',  ( -0.2965624338261537152, 4.505027248459144928, 0.09917050682623472502 ) ) ;
#7066 = VECTOR ( 'NONE', #9256, 39.37007874015748143 ) ;
#7067 = EDGE_CURVE ( 'NONE', #4071, #10339, #1674, .T. ) ;
#7068 = APPROVAL_ROLE ( '' ) ;
#7069 = CARTESIAN_POINT ( 'NONE',  ( -0.1688124736068475629, -0.2196335248263224516, -0.06558227484231513027 ) ) ;
#7070 = CARTESIAN_POINT ( 'NONE',  ( -0.1954553509668046918, -0.1954553509668046640, 0.3175000000000037237 ) ) ;
#7071 = CARTESIAN_POINT ( 'NONE',  ( 0.2819296736111110979, 3.950083333409199149, -3.452642723725051716E-17 ) ) ;
#7072 = CYLINDRICAL_SURFACE ( 'NONE', #10336, 0.3125000000000000000 ) ;
#7073 = LINE ( 'NONE', #1460, #7066 ) ;
#7074 = CARTESIAN_POINT ( 'NONE',  ( -0.2764156081756484196, 1.692557448933383907E-17, 0.3730555555555596925 ) ) ;
#7075 = CARTESIAN_POINT ( 'NONE',  ( -0.3613381517857143232, 0.1151785713310290032, -0.1174058825155741004 ) ) ;
#7076 = CARTESIAN_POINT ( 'NONE',  ( 0.2819296736111110979, 0.1465277777019111383, 0.000000000000000000 ) ) ;
#7077 = CARTESIAN_POINT ( 'NONE',  ( 0.4687500000000002776, 0.2172212470101570203, 0.07046416248101895763 ) ) ;
#7078 = CARTESIAN_POINT ( 'NONE',  ( -0.2088978631689275278, 0.3995044321532407738, -0.7203268866154032279 ) ) ;
#7079 = DIRECTION ( 'NONE',  ( 0.000000000000000000, -1.000000000000000000, 0.000000000000000000 ) ) ;
#7080 = CARTESIAN_POINT ( 'NONE',  ( 0.000000000000000000, 0.2764156081756484196, -0.02972222222222129645 ) ) ;
#7081 = VERTEX_POINT ( 'NONE', #24100 ) ;
#7082 = ORIENTED_EDGE ( 'NONE', *, *, #6985, .T. ) ;
#7083 = CARTESIAN_POINT ( 'NONE',  ( -0.06335377612981435425, 0.09459806137332689435, 0.4000000000000000777 ) ) ;
#7084 = CARTESIAN_POINT ( 'NONE',  ( -3.827021247335479543E-17, -0.3125000000000000000, 0.01888888888889002707 ) ) ;
#7085 = CARTESIAN_POINT ( 'NONE',  ( 0.2206173157302027676, 0.1222222222222218990, 0.2206173157302028787 ) ) ;
#7086 = CARTESIAN_POINT ( 'NONE',  ( -0.1993543840281266355, 3.762583333409198705, 0.1993543840281267465 ) ) ;
#7087 = CARTESIAN_POINT ( 'NONE',  ( -0.3613381517857144343, 0.05089285704531475163, 0.1174058825155740171 ) ) ;
#7088 = CARTESIAN_POINT ( 'NONE',  ( -0.2819296736111110424, 4.529944444520310753, -0.1167790944451423119 ) ) ;
#7089 = CARTESIAN_POINT ( 'NONE',  ( 0.4687500000000003886, -0.2922835737772481735, 0.06112444011295372487 ) ) ;
#7090 = EDGE_CURVE ( 'NONE', #15406, #13943, #10952, .T. ) ;
#7091 = DIRECTION ( 'NONE',  ( 0.000000000000000000, 0.000000000000000000, 1.000000000000000000 ) ) ;
#7092 = EDGE_CURVE ( 'NONE', #10191, #18764, #8970, .T. ) ;
#7093 = EDGE_LOOP ( 'NONE', ( #6376, #19796, #19819, #15167, #17780, #15566 ) ) ;
#7094 = EDGE_CURVE ( 'NONE', #3584, #13967, #6939, .T. ) ;
#7095 = CARTESIAN_POINT ( 'NONE',  ( 0.1236067977499789028, 0.3857142857142856207, 0.3804226065180614791 ) ) ;
#7096 = CARTESIAN_POINT ( 'NONE',  ( -0.1993543840281266355, 5.193138888964753619, 0.1993543840281267465 ) ) ;
#7097 = DIRECTION ( 'NONE',  ( -0.000000000000000000, -1.000000000000000000, -0.000000000000000000 ) ) ;
#7098 = EDGE_CURVE ( 'NONE', #16665, #20411, #9126, .T. ) ;
#7099 = CARTESIAN_POINT ( 'NONE',  ( 0.2472135954999579166, 0.2374999998049151795, 0.3402603233408160732 ) ) ;
#7100 = CARTESIAN_POINT ( 'NONE',  ( -0.3119999999999999996, 0.2090277777777774237, -0.1292346314604056745 ) ) ;
#7101 = CARTESIAN_POINT ( 'NONE',  ( 5.178964085587577574E-17, 4.922305555631420582, 0.2819296736111110979 ) ) ;
#7102 = APPROVAL_STATUS ( 'not_yet_approved' ) ;
#7103 = CARTESIAN_POINT ( 'NONE',  ( -0.1562568192738307826, 4.066946061297420201, 0.2700551682292786082 ) ) ;
#7104 = DIRECTION ( 'NONE',  ( 0.000000000000000000, 0.000000000000000000, -1.000000000000000000 ) ) ;
#7105 = ORIENTED_EDGE ( 'NONE', *, *, #15845, .F. ) ;
#7106 = CARTESIAN_POINT ( 'NONE',  ( -0.2819296736111110424, 0.2958333332574666907, -0.1167790944451423396 ) ) ;
#7107 = CARTESIAN_POINT ( 'NONE',  ( 0.1167790944451423257, 0.05972222214635558579, -0.2819296736111110424 ) ) ;
#7108 = CARTESIAN_POINT ( 'NONE',  ( 0.000000000000000000, 3.700000000000000622, -0.7199999999999994182 ) ) ;
#7109 = CARTESIAN_POINT ( 'NONE',  ( -1.399103805173478513E-17, 0.7678277469539112055, -1.002669935482285890 ) ) ;
#7110 = CARTESIAN_POINT ( 'NONE',  ( -0.2472135954999579999, 0.01785714285714282493, 0.3402603233408159622 ) ) ;
#7111 = CARTESIAN_POINT ( 'NONE',  ( -0.2230971623002954152, -0.2230971623002953874, -0.04187499999999937106 ) ) ;
#7112 = CIRCLE ( 'NONE', #2448, 0.3119999999999999996 ) ;
#7113 = EDGE_CURVE ( 'NONE', #22483, #10834, #16609, .T. ) ;
#7114 = ADVANCED_FACE ( 'NONE', ( #2168 ), #22232, .F. ) ;
#7115 = DIRECTION ( 'NONE',  ( 0.000000000000000000, 0.000000000000000000, -1.000000000000000000 ) ) ;
#7116 = CARTESIAN_POINT ( 'NONE',  ( 1.109470958122166229, 2.291712385858714285, -1.012998853824579104 ) ) ;
#7117 = CARTESIAN_POINT ( 'NONE',  ( -0.2819296736111110979, 4.588972222298088433, 0.000000000000000000 ) ) ;
#7118 = LINE ( 'NONE', #8114, #8532 ) ;
#7119 = CARTESIAN_POINT ( 'NONE',  ( -0.1167790944451423535, 5.043833333409199149, 0.2819296736111110424 ) ) ;
#7120 = CARTESIAN_POINT ( 'NONE',  ( -0.7171867353193368544, 0.9548081934128058723, 2.866728992292166378 ) ) ;
#7121 = CARTESIAN_POINT ( 'NONE',  ( 0.03947139886607073378, 3.764953234593765519, -0.3096039074880256314 ) ) ;
#7122 = CARTESIAN_POINT ( 'NONE',  ( 0.1720740510253924160, 0.05226575782620486443, 0.2482834776946442890 ) ) ;
#7123 = CARTESIAN_POINT ( 'NONE',  ( -0.2021572709300195614, 0.4370510722512948587, 0.07439726544911813566 ) ) ;
#7124 = CARTESIAN_POINT ( 'NONE',  ( 0.3119999999999999996, 4.252166666818399499, -3.820898013339742174E-17 ) ) ;
#7125 = CARTESIAN_POINT ( 'NONE',  ( -0.1167790944451423119, 4.523000000075866112, -0.2819296736111110979 ) ) ;
#7126 = CARTESIAN_POINT ( 'NONE',  ( -0.2819296736111110979, 3.852861111186976828, 0.000000000000000000 ) ) ;
#7127 = EDGE_LOOP ( 'NONE', ( #12755, #17092, #16007, #6770 ) ) ;
#7128 = AXIS2_PLACEMENT_3D ( 'NONE', #20879, #3820, #11263 ) ;
#7129 = ADVANCED_FACE ( 'NONE', ( #22760 ), #15096, .F. ) ;
#7130 = ORIENTED_EDGE ( 'NONE', *, *, #7067, .F. ) ;
#7131 = ORIENTED_EDGE ( 'NONE', *, *, #14186, .T. ) ;
#7132 = PERSON_AND_ORGANIZATION ( #15518, #2538 ) ;
#7133 = CARTESIAN_POINT ( 'NONE',  ( -0.03811151966973166244, -0.3039168590976487061, 0.4175033535898823311 ) ) ;
#7134 = CARTESIAN_POINT ( 'NONE',  ( -0.2496812655993395358, 4.940926318456405397, -0.1915063317200945969 ) ) ;
#7135 = CARTESIAN_POINT ( 'NONE',  ( 0.000000000000000000, 0.4202679491924311561, 0.000000000000000000 ) ) ;
#7136 = ORIENTED_EDGE ( 'NONE', *, *, #19558, .T. ) ;
#7137 = CARTESIAN_POINT ( 'NONE',  ( 0.3119999999999998885, 0.2298611109593782231, 0.1292346314604058410 ) ) ;
#7138 = CARTESIAN_POINT ( 'NONE',  ( 0.7919466436700954848, 0.05000000000000028727, -2.986000000000000210 ) ) ;
#7139 = CARTESIAN_POINT ( 'NONE',  ( -0.2684960426425861968, 5.119940279400660543, 0.1531817516059036377 ) ) ;
#7140 = PLANE ( 'NONE',  #1397 ) ;
#7141 = CARTESIAN_POINT ( 'NONE',  ( 0.2055726870590093569, 0.3152965443106340304, -0.7212806285457649125 ) ) ;
#7142 =( BOUNDED_CURVE ( )  B_SPLINE_CURVE ( 2, ( #9898, #19394, #23041, #23155, #2575, #13919, #4394, #8053, #15502 ),
 .UNSPECIFIED., .F., .T. ) 
 B_SPLINE_CURVE_WITH_KNOTS ( ( 3, 2, 2, 2, 3 ),
 ( 0.1145833333333333148, 0.1249999999999999722, 0.1354166666666667407, 0.1458333333333333703, 0.1562500000000000278 ),
 .UNSPECIFIED. ) 
 CURVE ( )  GEOMETRIC_REPRESENTATION_ITEM ( )  RATIONAL_B_SPLINE_CURVE ( ( 1.000000000000000444, 0.9238795325112862944, 1.000000000000000000, 0.9238795325112867385, 1.000000000000000000, 0.9238795325112867385, 1.000000000000000000, 0.9238795325112865164, 1.000000000000000222 ) ) 
 REPRESENTATION_ITEM ( '' )  );
#7143 = ORIENTED_EDGE ( 'NONE', *, *, #15315, .F. ) ;
#7144 =( BOUNDED_CURVE ( )  B_SPLINE_CURVE ( 2, ( #16371, #14790, #22206, #1840, #6, #15024, #22449, #16492, #12847 ),
 .UNSPECIFIED., .F., .F. ) 
 B_SPLINE_CURVE_WITH_KNOTS ( ( 3, 2, 2, 2, 3 ),
 ( 0.3124999999999999445, 0.3169642857142856429, 0.3214285714285713969, 0.3258928571428570953, 0.3303571428571427937 ),
 .UNSPECIFIED. ) 
 CURVE ( )  GEOMETRIC_REPRESENTATION_ITEM ( )  RATIONAL_B_SPLINE_CURVE ( ( 1.000000000000000888, 0.9238795325112857393, 1.000000000000000000, 0.9238795325112867385, 1.000000000000000000, 0.9238795325112867385, 1.000000000000000000, 0.9238795325112877377, 0.9999999999999990008 ) ) 
 REPRESENTATION_ITEM ( '' )  );
#7145 = DIRECTION ( 'NONE',  ( 7.284927983104698760E-15, -1.000000000000000000, -3.642463991552349380E-15 ) ) ;
#7146 = CARTESIAN_POINT ( 'NONE',  ( 0.000000000000000000, 0.2764156081756484196, 0.2411111111111142458 ) ) ;
#7147 = VECTOR ( 'NONE', #14018, 39.37007874015748854 ) ;
#7148 = CARTESIAN_POINT ( 'NONE',  ( -0.1167790944451423257, 4.120222222298087544, -0.2819296736111110424 ) ) ;
#7149 = CARTESIAN_POINT ( 'NONE',  ( -0.2819296736111110979, 5.127166666742532186, -0.1167790944451422980 ) ) ;
#7150 = CARTESIAN_POINT ( 'NONE',  ( -0.4687500000000004441, 0.1740113748017589612, 0.07813285960791813145 ) ) ;
#7151 = CARTESIAN_POINT ( 'NONE',  ( -0.1698811246234971650, 4.111524471938507119, -3.199085301159788841 ) ) ;
#7152 = CARTESIAN_POINT ( 'NONE',  ( -0.2206173157302028232, 4.043833333333332725, -0.2206173157302028232 ) ) ;
#7153 = CARTESIAN_POINT ( 'NONE',  ( 5.731347020009612645E-17, 4.960500000151731648, 0.3119999999999999996 ) ) ;
#7154 = CARTESIAN_POINT ( 'NONE',  ( 0.3102322028195323989, 4.806806770341049528, 0.03330294158711297886 ) ) ;
#7155 = CARTESIAN_POINT ( 'NONE',  ( -0.3119999999999998885, 4.165361111111110404, 0.1292346314604058410 ) ) ;
#7156 = EDGE_LOOP ( 'NONE', ( #21680, #10821, #13322, #12996 ) ) ;
#7157 = CARTESIAN_POINT ( 'NONE',  ( -0.09675901534512296176, 0.05896212819178082293, 0.2930612987570491157 ) ) ;
#7158 = ORIENTED_EDGE ( 'NONE', *, *, #14535, .T. ) ;
#7159 = CIRCLE ( 'NONE', #21186, 0.3119999999999999996 ) ;
#7160 = CARTESIAN_POINT ( 'NONE',  ( -0.3155070326520292845, 1.931923388228935888E-17, 0.2879861111111147731 ) ) ;
#7161 = CARTESIAN_POINT ( 'NONE',  ( 0.3613381517857143232, 0.3687499999024574926, 0.000000000000000000 ) ) ;
#7162 = CARTESIAN_POINT ( 'NONE',  ( 0.06335377612981431261, 0.05888377565904120980, -0.4000000000000000777 ) ) ;
#7163 = CARTESIAN_POINT ( 'NONE',  ( 0.2233192592356399164, 0.4116071427596004750, 0.3073725909049500604 ) ) ;
#7164 = CARTESIAN_POINT ( 'NONE',  ( 0.1993543840281266910, 0.2784722221463555858, -0.1993543840281266910 ) ) ;
#7165 = CARTESIAN_POINT ( 'NONE',  ( -0.2764156081756484196, -0.1144950937579609362, 0.1543055555555579716 ) ) ;
#7166 = CARTESIAN_POINT ( 'NONE',  ( 0.1993543840281267465, 5.109805555631420582, 0.1993543840281266633 ) ) ;
#7167 = CARTESIAN_POINT ( 'NONE',  ( 0.3064354089977339157, 4.472750180103851392, 0.05870368663529628578 ) ) ;
#7168 = ORIENTED_EDGE ( 'NONE', *, *, #13359, .F. ) ;
#7169 = CARTESIAN_POINT ( 'NONE',  ( 0.1167790944451422702, 4.779944444520309865, -0.2819296736111110424 ) ) ;
#7170 = CARTESIAN_POINT ( 'NONE',  ( 0.000000000000000000, 5.384999999999999787, 0.000000000000000000 ) ) ;
#7171 = CARTESIAN_POINT ( 'NONE',  ( -2.750539236387841874E-07, 4.266055563097283176, -0.3119999999998787632 ) ) ;
#7172 = CARTESIAN_POINT ( 'NONE',  ( 0.1292346314604009005, 4.068138888888888083, 0.3120000000000048845 ) ) ;
#7173 = FACE_OUTER_BOUND ( 'NONE', #15300, .T. ) ;
#7174 = CARTESIAN_POINT ( 'NONE',  ( -0.2206173157302028232, 4.710499999999999687, -0.2206173157302028232 ) ) ;
#7175 = CARTESIAN_POINT ( 'NONE',  ( 0.1634417798997719051, 5.205158050261544211, 0.2312413009345976878 ) ) ;
#7176 = CARTESIAN_POINT ( 'NONE',  ( -0.2819296736111110979, 4.071611111186976828, -0.1167790944451422980 ) ) ;
#7177 = AXIS2_PLACEMENT_3D ( 'NONE', #8311, #10284, #17707 ) ;
#7178 = CARTESIAN_POINT ( 'NONE',  ( -0.2819296736111110424, 3.759111111186976828, 0.1167790944451424923 ) ) ;
#7179 = CARTESIAN_POINT ( 'NONE',  ( 0.1028766551507927507, 4.040942783538628902, -0.2950564953585517736 ) ) ;
#7180 = CC_DESIGN_PERSON_AND_ORGANIZATION_ASSIGNMENT ( #19620, #8281, ( #6872 ) ) ;
#7181 = LINE ( 'NONE', #5342, #37 ) ;
#7182 = ORIENTED_EDGE ( 'NONE', *, *, #2163, .F. ) ;
#7183 = ORIENTED_EDGE ( 'NONE', *, *, #6672, .F. ) ;
#7184 = CARTESIAN_POINT ( 'NONE',  ( -0.003366903179265029553, -0.5383683782340863422, 0.05892738626661211260 ) ) ;
#7185 = CARTESIAN_POINT ( 'NONE',  ( -1.726321361862525858E-17, 4.227861111186976828, -0.2819296736111110979 ) ) ;
#7186 = CARTESIAN_POINT ( 'NONE',  ( -0.01087916929289088099, 4.488590625638971154, -0.3118577123740120527 ) ) ;
#7187 = CARTESIAN_POINT ( 'NONE',  ( -0.2085087158398496454, -0.1823754829287230206, -0.06558227484231535231 ) ) ;
#7188 = CARTESIAN_POINT ( 'NONE',  ( 0.000000000000000000, 0.2764156081756484196, 0.1300000000000022249 ) ) ;
#7189 = LINE ( 'NONE', #10854, #8368 ) ;
#7190 = CARTESIAN_POINT ( 'NONE',  ( -2.266361716303445225E-16, 4.432722222374099630, -0.3119999999999999996 ) ) ;
#7191 = CARTESIAN_POINT ( 'NONE',  ( -0.2764156081756484196, -0.1144950937579609362, 0.3765277777777819579 ) ) ;
#7192 = CARTESIAN_POINT ( 'NONE',  ( -0.3613381517857143232, 0.3294642856167431799, -0.1174058825155741004 ) ) ;
#7193 = CARTESIAN_POINT ( 'NONE',  ( -0.1167790944451424368, 0.1847222221463556413, 0.2819296736111110424 ) ) ;
#7194 = CARTESIAN_POINT ( 'NONE',  ( 0.008932132220340730649, 3.876926249342690145, -0.3118903982160737831 ) ) ;
#7195 = DIRECTION ( 'NONE',  ( -0.000000000000000000, -1.000000000000000000, -0.000000000000000000 ) ) ;
#7196 = ADVANCED_FACE ( 'NONE', ( #207 ), #2525, .F. ) ;
#7197 = CARTESIAN_POINT ( 'NONE',  ( -0.03517071929010351372, 0.1583405707270942042, -0.7492072654479503546 ) ) ;
#7198 = CARTESIAN_POINT ( 'NONE',  ( 0.1954553509668047195, 0.1954553509668046085, 0.07444444444444621445 ) ) ;
#7199 = ORIENTED_EDGE ( 'NONE', *, *, #14895, .T. ) ;
#7200 = CARTESIAN_POINT ( 'NONE',  ( 0.1988757138996042617, 3.752970977545328157, -0.2404006040361021113 ) ) ;
#7201 = CARTESIAN_POINT ( 'NONE',  ( 0.4593747947243453367, 0.02264684698529824056, 0.4343753230511080421 ) ) ;
#7202 = CARTESIAN_POINT ( 'NONE',  ( 1.910449006669871087E-17, -0.02361111111111144356, -0.3119999999999999996 ) ) ;
#7203 = CARTESIAN_POINT ( 'NONE',  ( -0.2819296736111110979, 3.922305555631421914, 0.000000000000000000 ) ) ;
#7204 = CARTESIAN_POINT ( 'NONE',  ( -0.1116596296178200276, 0.1330357141881718663, 0.3436530038418508792 ) ) ;
#7205 = VERTEX_POINT ( 'NONE', #22519 ) ;
#7206 = EDGE_CURVE ( 'NONE', #19663, #20305, #3475, .T. ) ;
#7207 = CARTESIAN_POINT ( 'NONE',  ( 0.1993543840281267465, 4.387583333409199149, 0.1993543840281266633 ) ) ;
#7208 = CYLINDRICAL_SURFACE ( 'NONE', #15887, 0.09499999999999995948 ) ;
#7209 = CARTESIAN_POINT ( 'NONE',  ( -0.3119999999999999996, 4.380638888888888083, -0.1292346314604056468 ) ) ;
#7210 = CARTESIAN_POINT ( 'NONE',  ( 0.01962962522499191176, 4.376629226301396614, -0.3119684076890694158 ) ) ;
#7211 = CARTESIAN_POINT ( 'NONE',  ( -0.1167790944451423257, 5.231333333409198261, -0.2819296736111110424 ) ) ;
#7212 = AXIS2_PLACEMENT_3D ( 'NONE', #23748, #16695, #7432 ) ;
#7213 = CARTESIAN_POINT ( 'NONE',  ( 0.2875779526214432003, 4.193046792779527188, 0.1220845629366733021 ) ) ;
#7214 =( NAMED_UNIT ( * ) PLANE_ANGLE_UNIT ( ) SI_UNIT ( $, .RADIAN. ) );
#7215 = CYLINDRICAL_SURFACE ( 'NONE', #5287, 0.3119999999999999996 ) ;
#7216 = CARTESIAN_POINT ( 'NONE',  ( 0.2918969027557590246, -0.06668494381002647298, -0.08811163115763034903 ) ) ;
#7217 = APPROVAL_PERSON_ORGANIZATION ( #14506, #18042, #18733 ) ;
#7218 = CARTESIAN_POINT ( 'NONE',  ( -0.1167790944451423119, 4.620222222298087544, -0.2819296736111110979 ) ) ;
#7219 = CALENDAR_DATE ( 2026, 7, 10 ) ;
#7220 = CARTESIAN_POINT ( 'NONE',  ( -0.1545212632259251595, 4.067003750745931789, 0.2710483404691284015 ) ) ;
#7221 = ADVANCED_FACE ( 'NONE', ( #10328 ), #21863, .F. ) ;
#7222 = CARTESIAN_POINT ( 'NONE',  ( 0.4749999999999999778, 3.700000000000000622, 2.908536147974959276E-17 ) ) ;
#7223 = CARTESIAN_POINT ( 'NONE',  ( -0.1167790944451422702, 0.3444444443685777402, -0.2819296736111110424 ) ) ;
#7224 = ADVANCED_FACE ( 'NONE', ( #14557 ), #23340, .T. ) ;
#7225 = ORIENTED_EDGE ( 'NONE', *, *, #17461, .T. ) ;
#7226 = VERTEX_POINT ( 'NONE', #8353 ) ;
#7227 = CARTESIAN_POINT ( 'NONE',  ( -0.1167790944451422702, 0.2333333332574666907, -0.2819296736111110424 ) ) ;
#7228 = CARTESIAN_POINT ( 'NONE',  ( -0.3119999999999999996, 4.325083333333332725, -0.1292346314604056468 ) ) ;
#7229 = CARTESIAN_POINT ( 'NONE',  ( -0.5116234456863466562, 0.6134519301839024275, 2.549370209580444691 ) ) ;
#7230 = AXIS2_PLACEMENT_3D ( 'NONE', #16285, #9325, #21766 ) ;
#7231 = CARTESIAN_POINT ( 'NONE',  ( -0.4000000000000000222, -0.06428571428571429325, -4.898587196589413075E-17 ) ) ;
#7232 = CARTESIAN_POINT ( 'NONE',  ( -0.2230971623002954152, -0.2230971623002953874, -0.09743055555555536762 ) ) ;
#7233 = DIRECTION ( 'NONE',  ( 0.000000000000000000, 0.000000000000000000, 1.000000000000000000 ) ) ;
#7234 = CARTESIAN_POINT ( 'NONE',  ( -0.2565705662273032872, 3.885668986695542060, -0.1775261799423144271 ) ) ;
#7235 = CARTESIAN_POINT ( 'NONE',  ( -0.1167790944451422702, 0.1083333332574667046, -0.2819296736111110424 ) ) ;
#7236 = CARTESIAN_POINT ( 'NONE',  ( 0.1993543840281267465, 4.554250000075866112, 0.1993543840281266633 ) ) ;
#7237 = CARTESIAN_POINT ( 'NONE',  ( 2.575339694675500462E-17, 0.1946428569477723081, -0.4205848896953069405 ) ) ;
#7238 = CARTESIAN_POINT ( 'NONE',  ( 0.03118581108655819195, 4.516944820282859929, 0.3111218374044668611 ) ) ;
#7239 = EDGE_CURVE ( 'NONE', #22475, #8827, #4700, .T. ) ;
#7240 = CARTESIAN_POINT ( 'NONE',  ( 0.1167790944451424368, 5.050777777853643791, 0.2819296736111110424 ) ) ;
#7241 = CARTESIAN_POINT ( 'NONE',  ( -0.2865907421542747691, 0.05024142792322828371, -0.09003034002162962901 ) ) ;
#7242 = CARTESIAN_POINT ( 'NONE',  ( 0.2959576967297150585, 3.749313823154953873, 0.1001818723666523803 ) ) ;
#7243 = LOCAL_TIME ( 21, 9, 13.00000000000000000, #403 ) ;
#7244 = LINE ( 'NONE', #7359, #5494 ) ;
#7245 = CARTESIAN_POINT ( 'NONE',  ( 0.09681669869989185939, 3.929937981323567087, -0.2975949584254778957 ) ) ;
#7246 = CARTESIAN_POINT ( 'NONE',  ( -0.3119999999999999996, 4.335500000151731648, 0.000000000000000000 ) ) ;
#7247 = CARTESIAN_POINT ( 'NONE',  ( 0.1993543840281267465, 4.498694444520309865, 0.1993543840281266633 ) ) ;
#7248 = CARTESIAN_POINT ( 'NONE',  ( 0.1167790944451424368, 3.870222222298087988, 0.2819296736111110424 ) ) ;
#7249 = VECTOR ( 'NONE', #22566, 39.37007874015748143 ) ;
#7250 = ORIENTED_EDGE ( 'NONE', *, *, #20260, .T. ) ;
#7251 = EDGE_LOOP ( 'NONE', ( #18276, #3353, #11940, #6835 ) ) ;
#7252 = DATE_TIME_ROLE ( 'creation_date' ) ;
#7253 = CARTESIAN_POINT ( 'NONE',  ( -0.1292346314604057300, 4.283416666666665762, 0.3119999999999998885 ) ) ;
#7254 = CARTESIAN_POINT ( 'NONE',  ( -0.3037294952134644288, 4.948996506944134843, 0.08224234445281884687 ) ) ;
#7255 = DIRECTION ( 'NONE',  ( 0.8660254037844383745, 0.5000000000000003331, 0.000000000000000000 ) ) ;
#7256 = LOCAL_TIME ( 21, 9, 13.00000000000000000, #14175 ) ;
#7257 = ORIENTED_EDGE ( 'NONE', *, *, #12814, .F. ) ;
#7258 = CARTESIAN_POINT ( 'NONE',  ( 0.3119999999999999996, 0.1812499998482670904, -0.1292346314604056468 ) ) ;
#7259 = CARTESIAN_POINT ( 'NONE',  ( 0.3613381517857143232, 0.4312499999024575481, 0.000000000000000000 ) ) ;
#7260 = CARTESIAN_POINT ( 'NONE',  ( -0.1930140748054549049, 3.716415235292884311, -0.2451613398821450296 ) ) ;
#7261 = CARTESIAN_POINT ( 'NONE',  ( 1.750236327630675537E-16, 0.08749999980491518503, 0.3999999999999999667 ) ) ;
#7262 = DIRECTION ( 'NONE',  ( -1.000000000000000000, 0.000000000000000000, 0.000000000000000000 ) ) ;
#7263 = VERTEX_POINT ( 'NONE', #690 ) ;
#7264 = CARTESIAN_POINT ( 'NONE',  ( -0.1116596296178200276, 0.2044642856167432909, 0.3436530038418508792 ) ) ;
#7265 = VECTOR ( 'NONE', #5631, 39.37007874015748143 ) ;
#7266 = CARTESIAN_POINT ( 'NONE',  ( 0.3042850080729309070, 5.083614731684491517, 0.07087365376649608362 ) ) ;
#7267 = CARTESIAN_POINT ( 'NONE',  ( -0.1954553509668046640, 0.1954553509668046918, 0.3036111111111147176 ) ) ;
#7268 = CARTESIAN_POINT ( 'NONE',  ( 5.178964085587577574E-17, 4.311194444520309865, 0.2819296736111110979 ) ) ;
#7269 = CARTESIAN_POINT ( 'NONE',  ( 0.2819296736111111534, 5.099388888964754507, 0.1167790944451422563 ) ) ;
#7270 = CARTESIAN_POINT ( 'NONE',  ( -0.09435543239133792337, 4.559812086079793048, -2.854670964936879329 ) ) ;
#7271 = CARTESIAN_POINT ( 'NONE',  ( -0.3076274917712982782, 4.225837578920637050, 0.05212383236253055607 ) ) ;
#7272 = CARTESIAN_POINT ( 'NONE',  ( 0.1292346314604056190, 3.811194444444443441, -0.3119999999999999996 ) ) ;
#7273 = CARTESIAN_POINT ( 'NONE',  ( -1.910449006669871087E-17, 4.932722222373954857, -0.3119999999999999996 ) ) ;
#7274 = CARTESIAN_POINT ( 'NONE',  ( 0.2916638615397387779, 4.804523324935893847, 0.1117996548601188078 ) ) ;
#7275 = CARTESIAN_POINT ( 'NONE',  ( 0.000000000000000000, 5.384999999999999787, -0.3119999999999999996 ) ) ;
#7276 = ORIENTED_EDGE ( 'NONE', *, *, #13343, .F. ) ;
#7277 = CARTESIAN_POINT ( 'NONE',  ( 0.1112748779815979916, 0.04093257519601814498, -0.2692499194552509523 ) ) ;
#7278 = VECTOR ( 'NONE', #5389, 39.37007874015748143 ) ;
#7279 = VERTEX_POINT ( 'NONE', #6295 ) ;
#7280 =( BOUNDED_CURVE ( )  B_SPLINE_CURVE ( 2, ( #12110, #17336, #2813, #629, #23279, #6593, #4755, #15390, #6108 ),
 .UNSPECIFIED., .F., .T. ) 
 B_SPLINE_CURVE_WITH_KNOTS ( ( 3, 2, 2, 2, 3 ),
 ( 0.8303571428571426827, 0.8348214285714283811, 0.8392857142857141906, 0.8437500000000000000, 0.8482142857142856984 ),
 .UNSPECIFIED. ) 
 CURVE ( )  GEOMETRIC_REPRESENTATION_ITEM ( )  RATIONAL_B_SPLINE_CURVE ( ( 1.000000000000003775, 0.9238795325112829637, 1.000000000000000000, 0.9238795325112867385, 1.000000000000000000, 0.9238795325112867385, 1.000000000000000000, 0.9238795325112867385, 1.000000000000000000 ) ) 
 REPRESENTATION_ITEM ( '' )  );
#7281 = CARTESIAN_POINT ( 'NONE',  ( 0.3155070326520292845, -5.795770164686806123E-17, 0.2046527777777807644 ) ) ;
#7282 = CARTESIAN_POINT ( 'NONE',  ( -0.1993543840281266910, 5.012583333409199149, -0.1993543840281266910 ) ) ;
#7283 =( BOUNDED_CURVE ( )  B_SPLINE_CURVE ( 2, ( #23738, #14873, #6937, #21806, #14501, #18155, #9735, #18881, #5825 ),
 .UNSPECIFIED., .F., .F. ) 
 B_SPLINE_CURVE_WITH_KNOTS ( ( 3, 2, 2, 2, 3 ),
 ( 0.4553571428571429602, 0.4598214285714286587, 0.4642857142857144126, 0.4687500000000001110, 0.4732142857142858094 ),
 .UNSPECIFIED. ) 
 CURVE ( )  GEOMETRIC_REPRESENTATION_ITEM ( )  RATIONAL_B_SPLINE_CURVE ( ( 0.9999999999999981126, 0.9238795325112886259, 1.000000000000000000, 0.9238795325112867385, 1.000000000000000000, 0.9238795325112867385, 1.000000000000000000, 0.9238795325112848511, 1.000000000000001998 ) ) 
 REPRESENTATION_ITEM ( '' )  );
#7284 = CARTESIAN_POINT ( 'NONE',  ( 0.2923287055106771337, 0.3580357141881718164, -0.2123892367102620249 ) ) ;
#7285 = CARTESIAN_POINT ( 'NONE',  ( 0.1993543840281266355, 0.3756944443685777957, 0.1993543840281267465 ) ) ;
#7286 = CARTESIAN_POINT ( 'NONE',  ( 0.1954553509668047195, 0.1954553509668046085, 0.2411111111111141903 ) ) ;
#7287 = ADVANCED_FACE ( 'NONE', ( #23103 ), #13865, .T. ) ;
#7288 = CARTESIAN_POINT ( 'NONE',  ( -0.1993543840281266355, 5.040361111186977716, 0.1993543840281267465 ) ) ;
#7289 = CARTESIAN_POINT ( 'NONE',  ( 0.3050023557400097785, 4.472545578696121460, 0.06570874416663827211 ) ) ;
#7290 = ORIENTED_EDGE ( 'NONE', *, *, #23927, .F. ) ;
#7291 = EDGE_CURVE ( 'NONE', #8965, #2744, #19576, .T. ) ;
#7292 = CARTESIAN_POINT ( 'NONE',  ( 0.1167790944451422702, 4.835500000075865223, -0.2819296736111110424 ) ) ;
#7293 = FACE_OUTER_BOUND ( 'NONE', #4585, .T. ) ;
#7294 = CARTESIAN_POINT ( 'NONE',  ( -1.910449006669871087E-17, 5.036888888888888971, -0.3119999999999999996 ) ) ;
#7295 = CARTESIAN_POINT ( 'NONE',  ( 0.1633221850526035690, 2.539511724522410611E-17, 0.3257820047251743789 ) ) ;
#7296 = CARTESIAN_POINT ( 'NONE',  ( 2.936000000000000387, -3.638933710489514981E-33, -2.591000000000000636 ) ) ;
#7297 = CARTESIAN_POINT ( 'NONE',  ( 0.2206173157302028787, 4.627166666666665762, 0.2206173157302027954 ) ) ;
#7298 = AXIS2_PLACEMENT_3D ( 'NONE', #813, #6417, #23346 ) ;
#7299 = CARTESIAN_POINT ( 'NONE',  ( -0.1993543840281266355, 4.082027777853643791, 0.1993543840281267465 ) ) ;
#7300 = LINE ( 'NONE', #14749, #20227 ) ;
#7301 = CARTESIAN_POINT ( 'NONE',  ( 0.1565020774999655861, 4.020729645363375404, 0.2706823387111469414 ) ) ;
#7302 = CARTESIAN_POINT ( 'NONE',  ( 0.3120000000000000551, 4.408416666666666650, 0.1292346314604056190 ) ) ;
#7303 = ORIENTED_EDGE ( 'NONE', *, *, #24055, .T. ) ;
#7304 = CARTESIAN_POINT ( 'NONE',  ( -0.1294417382415922746, -0.3125000000000000000, 0.1265277777777797930 ) ) ;
#7305 = CARTESIAN_POINT ( 'NONE',  ( -0.1730627168398009008, 4.121933759322424784, 0.2596022278612341583 ) ) ;
#7306 = CARTESIAN_POINT ( 'NONE',  ( 0.3119999999999999996, 0.07708333333333300397, -0.1292346314604056468 ) ) ;
#7307 = CARTESIAN_POINT ( 'NONE',  ( -0.2764156081756484196, 1.692557448933383907E-17, 0.2550000000000032241 ) ) ;
#7308 = VECTOR ( 'NONE', #1421, 39.37007874015748143 ) ;
#7309 = CARTESIAN_POINT ( 'NONE',  ( -0.3125000000000000000, 1.913510623667739771E-17, 0.2897222222222258226 ) ) ;
#7310 = CARTESIAN_POINT ( 'NONE',  ( 0.4673607484394255440, 0.2845795129072107299, 0.04287645741408792344 ) ) ;
#7311 = CC_DESIGN_PERSON_AND_ORGANIZATION_ASSIGNMENT ( #4328, #20799, ( #5255 ) ) ;
#7312 = DIRECTION ( 'NONE',  ( -0.000000000000000000, -1.000000000000000000, -0.000000000000000000 ) ) ;
#7313 = CARTESIAN_POINT ( 'NONE',  ( 0.2923287055106771337, 0.2187499999024575537, 0.2123892367102621359 ) ) ;
#7314 = CARTESIAN_POINT ( 'NONE',  ( 0.1993543840281266910, 0.2645833332574666907, -0.1993543840281266910 ) ) ;
#7315 = CARTESIAN_POINT ( 'NONE',  ( 0.002232267356213628925, 3.877106664906796230, -0.3119931564268053625 ) ) ;
#7316 = CARTESIAN_POINT ( 'NONE',  ( 3.820898013339742174E-17, 5.384999999999999787, 0.3119999999999999996 ) ) ;
#7317 = CARTESIAN_POINT ( 'NONE',  ( 9.184120737366631376E-17, 0.1556215347031258134, -0.7500000000000001110 ) ) ;
#7318 = CARTESIAN_POINT ( 'NONE',  ( -0.1144950937579609918, -0.2764156081756484196, -0.005416666666665557496 ) ) ;
#7319 = ORIENTED_EDGE ( 'NONE', *, *, #6958, .F. ) ;
#7320 = ORIENTED_EDGE ( 'NONE', *, *, #18698, .T. ) ;
#7321 = CARTESIAN_POINT ( 'NONE',  ( -0.2338243153676845543, 5.099281701770390640, -0.2058997526750516449 ) ) ;
#7322 = CARTESIAN_POINT ( 'NONE',  ( 0.4687500000000003331, 0.02249286784990170429, 0.4289627432666881512 ) ) ;
#7323 = CARTESIAN_POINT ( 'NONE',  ( 0.2819296736111110979, 0.5909722221463555858, 0.000000000000000000 ) ) ;
#7324 = CARTESIAN_POINT ( 'NONE',  ( 0.1797082215028593943, 3.735609866510083865, -0.2172309738199109941 ) ) ;
#7325 = CARTESIAN_POINT ( 'NONE',  ( -0.3613381517857143232, 0.1901785713310290282, -4.425116109941954795E-17 ) ) ;
#7326 = CARTESIAN_POINT ( 'NONE',  ( 0.2819296736111110979, 4.450083333409199149, -3.452642723725051716E-17 ) ) ;
#7327 = CARTESIAN_POINT ( 'NONE',  ( 0.2206173157302028787, 4.960499999999998799, 0.2206173157302027954 ) ) ;
#7328 = CARTESIAN_POINT ( 'NONE',  ( 2.936000000000001720, 2.740000000000000213, 0.000000000000000000 ) ) ;
#7329 = ORIENTED_EDGE ( 'NONE', *, *, #4837, .F. ) ;
#7330 = VECTOR ( 'NONE', #414, 39.37007874015748143 ) ;
#7331 = CARTESIAN_POINT ( 'NONE',  ( 0.04079027354135526806, 4.350485889367855741, 0.3119999945730878022 ) ) ;
#7332 = CARTESIAN_POINT ( 'NONE',  ( 0.1167790944451424368, 4.925777777853642903, 0.2819296736111110424 ) ) ;
#7333 = EDGE_CURVE ( 'NONE', #20229, #1954, #13983, .T. ) ;
#7334 = DIRECTION ( 'NONE',  ( -0.000000000000000000, -1.000000000000000000, -0.000000000000000000 ) ) ;
#7335 = DIRECTION ( 'NONE',  ( -0.000000000000000000, 1.000000000000000000, -0.000000000000000000 ) ) ;
#7336 = CARTESIAN_POINT ( 'NONE',  ( 0.2819296736111110979, 4.769527777853642903, -3.452642723725051716E-17 ) ) ;
#7337 = ADVANCED_FACE ( 'NONE', ( #10092 ), #22929, .F. ) ;
#7338 = CARTESIAN_POINT ( 'NONE',  ( 0.000000000000000000, 0.1199999999999999956, 0.000000000000000000 ) ) ;
#7339 = CARTESIAN_POINT ( 'NONE',  ( -5.731347020009612645E-17, 0.4416666665149336923, 0.3119999999999999996 ) ) ;
#7340 = CARTESIAN_POINT ( 'NONE',  ( 1.726321361862525858E-17, 0.5631944443685776847, -0.2819296736111110979 ) ) ;
#7341 = EDGE_LOOP ( 'NONE', ( #10246, #4901, #19695, #11869, #10196 ) ) ;
#7342 = ORIENTED_EDGE ( 'NONE', *, *, #14854, .T. ) ;
#7343 = CARTESIAN_POINT ( 'NONE',  ( 0.1167790944451423257, 0.2263888888130222710, -0.2819296736111110424 ) ) ;
#7344 = CARTESIAN_POINT ( 'NONE',  ( -0.1292346314604081170, 4.318138888888888083, -0.3119999999999975016 ) ) ;
#7345 = CARTESIAN_POINT ( 'NONE',  ( -0.2805147388977641820, 5.200218985593472176, -0.05155921707341403620 ) ) ;
#7346 = CARTESIAN_POINT ( 'NONE',  ( -0.1236067977499789583, 0.06428571428571425161, -0.3804226065180614791 ) ) ;
#7347 = CARTESIAN_POINT ( 'NONE',  ( 0.3155070326520292845, -5.795770164686806123E-17, -0.02104166666666586888 ) ) ;
#7348 = CARTESIAN_POINT ( 'NONE',  ( -0.2721904660997562231, -0.3841166384917365506, 0.07944544255958575774 ) ) ;
#7349 = CARTESIAN_POINT ( 'NONE',  ( -0.3125022104525487232, 3.890849970558711401, -0.006219195744223885054 ) ) ;
#7350 = B_SPLINE_CURVE_WITH_KNOTS ( 'NONE', 3,
 ( #13534, #822, #23235, #15582, #20828, #6307, #23006, #19472, #11813, #15466, #4477, #13760, #2768, #20948, #17645, #4120, #933, #17530, #19003, #17177, #11941, #19116, #22891, #15345, #6185, #19358, #11578, #7893, #4239, #8251, #15702, #13648, #2302, #8364, #9738, #462, #583, #2421, #23117, #19233, #21066, #2539, #9862, #6427, #13880, #21310, #17291, #20079, #1545, #2882, #21902, #7037 ),
 .UNSPECIFIED., .F., .F.,
 ( 4, 2, 1, 1, 1, 1, 1, 1, 2, 2, 2, 2, 2, 2, 2, 2, 2, 2, 1, 1, 2, 2, 2, 2, 2, 2, 2, 2, 2, 4 ),
 ( 0.3380880081932458592, 0.3380924783650609000, 0.3380969485368759408, 0.3381058888805060225, 0.3381237695677661859, 0.3381595309422865125, 0.3382310536913272214, 0.3383740991894085282, 0.3386601901855712526, 0.3392323721778965906, 0.3403767361625473220, 0.3415211001471980534, 0.3426654641318487848, 0.3438098281164995162, 0.3443820101088249097, 0.3446681011049875787, 0.3446859817922477420, 0.3447038624795079054, 0.3447396238540282321, 0.3448111466030689409, 0.3449541921011502477, 0.3472429200704517105, 0.3495316480397531178, 0.3518203760090545251, 0.3541091039783559324, 0.3552534679630066083, 0.3553965134610879706, 0.3555395589591693328, 0.3558256499553320018, 0.3563978319476573398 ),
 .UNSPECIFIED. ) ;
#7351 = CARTESIAN_POINT ( 'NONE',  ( 1.726321361862525858E-17, -0.006250000075866632768, -0.2819296736111110979 ) ) ;
#7352 = CARTESIAN_POINT ( 'NONE',  ( 0.2819296736111110979, 4.446611111186976828, 0.1167790944451422425 ) ) ;
#7354 = B_SPLINE_CURVE_WITH_KNOTS ( 'NONE', 3,
 ( #23615, #13042, #9242, #20220, #3508, #6930 ),
 .UNSPECIFIED., .F., .F.,
 ( 4, 2, 4 ),
 ( 0.05028785581520123227, 0.1127878554948266582, 0.1752878551744520841 ),
 .UNSPECIFIED. ) ;
#7353 = CARTESIAN_POINT ( 'NONE',  ( 0.3236067977499790249, 0.1839285712334866596, -0.2351141009169892826 ) ) ;
#7355 = CARTESIAN_POINT ( 'NONE',  ( 0.01477765123391010932, 4.543413721529206306, -0.3116996714995854401 ) ) ;
#7356 = CARTESIAN_POINT ( 'NONE',  ( 0.1167790944451424368, 5.106333333409198261, 0.2819296736111110424 ) ) ;
#7357 = CARTESIAN_POINT ( 'NONE',  ( 0.1167790944451422702, 4.446611111186976828, -0.2819296736111110979 ) ) ;
#7358 = CARTESIAN_POINT ( 'NONE',  ( 0.2531481986011811514, 3.757757936612477145, -0.1838958115507471347 ) ) ;
#7359 = CARTESIAN_POINT ( 'NONE',  ( 0.4453125000000000000, 0.000000000000000000, 0.4425000000000000044 ) ) ;
#7360 = CARTESIAN_POINT ( 'NONE',  ( 0.1297984762942410164, 3.908702258813368857, 0.2857640727182840790 ) ) ;
#7361 = CARTESIAN_POINT ( 'NONE',  ( -1.910449006669871087E-17, 4.099388889040620931, -0.3119999999999999996 ) ) ;
#7362 = CARTESIAN_POINT ( 'NONE',  ( 5.178964085587577574E-17, 4.436194444520310753, 0.2819296736111110979 ) ) ;
#7363 = CARTESIAN_POINT ( 'NONE',  ( 0.2819296736111110424, 3.828555555631421026, -0.1167790944451423396 ) ) ;
#7364 = CIRCLE ( 'NONE', #6975, 0.01875000000000001318 ) ;
#7365 = EDGE_LOOP ( 'NONE', ( #18810, #8995, #1558, #14276 ) ) ;
#7366 = EDGE_LOOP ( 'NONE', ( #4734, #20179, #23700 ) ) ;
#7367 = DATE_AND_TIME ( #22117, #22021 ) ;
#7368 = CARTESIAN_POINT ( 'NONE',  ( 0.06232504194019378163, -0.3017193634690418791, 0.4192984290766904043 ) ) ;
#7369 = EDGE_CURVE ( 'NONE', #11100, #7025, #2281, .T. ) ;
#7370 = CARTESIAN_POINT ( 'NONE',  ( -0.08174960291637467513, 4.935080742073520099, -0.3038624884746509713 ) ) ;
#7371 = FACE_OUTER_BOUND ( 'NONE', #3653, .T. ) ;
#7372 = VERTEX_POINT ( 'NONE', #21980 ) ;
#7373 = CARTESIAN_POINT ( 'NONE',  ( -5.731347020009612645E-17, 0.5527777776260448528, 0.3119999999999999996 ) ) ;
#7374 = DIRECTION ( 'NONE',  ( -0.000000000000000000, 1.000000000000000000, -0.000000000000000000 ) ) ;
#7375 = CARTESIAN_POINT ( 'NONE',  ( -0.1997712965817471376, 3.716669753339185700, -0.2396573947470825861 ) ) ;
#7376 = FACE_OUTER_BOUND ( 'NONE', #18987, .T. ) ;
#7377 = DIRECTION ( 'NONE',  ( 0.000000000000000000, 0.000000000000000000, -1.000000000000000000 ) ) ;
#7378 = EDGE_LOOP ( 'NONE', ( #23948, #5913, #3011, #4652 ) ) ;
#7379 = CARTESIAN_POINT ( 'NONE',  ( 0.2923287055106771337, 0.07589285704531474608, 0.2123892367102621359 ) ) ;
#7380 = VECTOR ( 'NONE', #14894, 39.37007874015748143 ) ;
#7381 = VERTEX_POINT ( 'NONE', #16388 ) ;
#7382 = CARTESIAN_POINT ( 'NONE',  ( 0.1969676853939942296, 5.093707226201246385, -0.2418488411147588502 ) ) ;
#7383 = CARTESIAN_POINT ( 'NONE',  ( -0.1144950937579609918, -0.2764156081756484196, 0.2098611111111139960 ) ) ;
#7384 = CARTESIAN_POINT ( 'NONE',  ( -0.2819296736111110424, 4.238277777853642903, -0.1167790944451423119 ) ) ;
#7385 = CARTESIAN_POINT ( 'NONE',  ( 0.1993543840281267465, 5.095916666742532186, 0.1993543840281266633 ) ) ;
#7386 = CARTESIAN_POINT ( 'NONE',  ( 0.3060165374364313129, -0.008786209580232379190, 0.4176832041030980047 ) ) ;
#7387 = CARTESIAN_POINT ( 'NONE',  ( -0.3094852631870094739, 4.225487789190556676, 0.03986035098601010268 ) ) ;
#7388 = CARTESIAN_POINT ( 'NONE',  ( -1.910449006669871087E-17, 3.759111111111109960, -0.3119999999999999996 ) ) ;
#7389 = CARTESIAN_POINT ( 'NONE',  ( 0.2206173157302028787, 5.023000000151731648, 0.2206173157302027954 ) ) ;
#7390 = CARTESIAN_POINT ( 'NONE',  ( 0.1167790944451422702, 5.127166666742532186, -0.2819296736111110979 ) ) ;
#7391 = EDGE_CURVE ( 'NONE', #18827, #11232, #8234, .T. ) ;
#7392 = ADVANCED_FACE ( 'NONE', ( #23796, #5153 ), #12618, .T. ) ;
#7393 = ADVANCED_FACE ( 'NONE', ( #13747 ), #12046, .T. ) ;
#7394 = LINE ( 'NONE', #5557, #19850 ) ;
#7395 = ORIENTED_EDGE ( 'NONE', *, *, #18460, .F. ) ;
#7396 = ADVANCED_BREP_SHAPE_REPRESENTATION ( '', ( #1208, #9127 ), #2138 ) ;
#7397 = CARTESIAN_POINT ( 'NONE',  ( 0.2793135105113299654, 0.03335568393651896363, 0.05007282442598128686 ) ) ;
#7398 = AXIS2_PLACEMENT_3D ( 'NONE', #19411, #17586, #1120 ) ;
#7399 = ORIENTED_EDGE ( 'NONE', *, *, #17718, .F. ) ;
#7400 = ADVANCED_FACE ( 'NONE', ( #923 ), #3325, .T. ) ;
#7401 = CARTESIAN_POINT ( 'NONE',  ( 0.1306872919485614071, -0.3155070326520293955, 0.3053472222222260446 ) ) ;
#7402 = CARTESIAN_POINT ( 'NONE',  ( 0.2819296736111110424, 5.106333333409198261, -0.1167790944451423396 ) ) ;
#7403 = ORIENTED_EDGE ( 'NONE', *, *, #22883, .T. ) ;
#7404 = CARTESIAN_POINT ( 'NONE',  ( 0.4622078388679876082, -0.2744100571732867588, 0.3892820121258429023 ) ) ;
#7405 = CARTESIAN_POINT ( 'NONE',  ( -0.3613381517857143232, 0.3830357141881717276, -0.1174058825155741004 ) ) ;
#7406 = CARTESIAN_POINT ( 'NONE',  ( -0.2819296736111111534, 0.3027777777019111660, 0.1167790944451422563 ) ) ;
#7407 = CARTESIAN_POINT ( 'NONE',  ( 0.2764156081756483641, -0.1144950937579611167, 0.2306944444444474218 ) ) ;
#7408 = CARTESIAN_POINT ( 'NONE',  ( 5.178964085587577574E-17, 4.880638888964754507, 0.2819296736111110979 ) ) ;
#7409 = CARTESIAN_POINT ( 'NONE',  ( 0.04280166039970490638, 4.487079570219966840, -0.3091224059445770722 ) ) ;
#7410 = CARTESIAN_POINT ( 'NONE',  ( 0.2819296736111110979, 4.877166666742533963, 0.1167790944451422425 ) ) ;
#7411 = CARTESIAN_POINT ( 'NONE',  ( 0.3860879860166477329, 3.066692553488282957, 2.740461747820544414 ) ) ;
#7412 = CIRCLE ( 'NONE', #9362, 0.3125000000000000000 ) ;
#7413 = CARTESIAN_POINT ( 'NONE',  ( -0.002403927698694708574, 4.266120144334736963, -0.3119999978808592478 ) ) ;
#7414 = CARTESIAN_POINT ( 'NONE',  ( -0.5116234456863466562, 0.9548081934128058723, 2.635972749958888528 ) ) ;
#7415 = LINE ( 'NONE', #7296, #21315 ) ;
#7416 = CARTESIAN_POINT ( 'NONE',  ( -0.1292346314604056745, 4.595916666666665762, -0.3119999999999999996 ) ) ;
#7417 = VECTOR ( 'NONE', #19637, 39.37007874015748854 ) ;
#7418 = CARTESIAN_POINT ( 'NONE',  ( -0.1993543840281266355, 3.970916666742532186, 0.1993543840281267465 ) ) ;
#7419 = CARTESIAN_POINT ( 'NONE',  ( 0.04820796449995154442, 5.072973651020436847, 0.3082531300064171864 ) ) ;
#7420 = CARTESIAN_POINT ( 'NONE',  ( 0.1561509399989899904, 4.039288193619596790, -0.2708485047170307025 ) ) ;
#7421 = DIRECTION ( 'NONE',  ( -0.000000000000000000, -1.000000000000000000, -0.000000000000000000 ) ) ;
#7422 = CARTESIAN_POINT ( 'NONE',  ( 0.2206173157302027954, 3.918833333333332281, -0.2206173157302028232 ) ) ;
#7423 = ORIENTED_EDGE ( 'NONE', *, *, #17379, .F. ) ;
#7424 =( BOUNDED_CURVE ( )  B_SPLINE_CURVE ( 2, ( #1427, #8855, #16299, #7155, #10938, #12658, #23711, #21780, #23834 ),
 .UNSPECIFIED., .F., .F. ) 
 B_SPLINE_CURVE_WITH_KNOTS ( ( 3, 2, 2, 2, 3 ),
 ( 0.7053571428571429047, 0.7098214285714286031, 0.7142857142857144126, 0.7187500000000001110, 0.7232142857142858094 ),
 .UNSPECIFIED. ) 
 CURVE ( )  GEOMETRIC_REPRESENTATION_ITEM ( )  RATIONAL_B_SPLINE_CURVE ( ( 1.000000000000000000, 0.9238795325112867385, 1.000000000000000000, 0.9238795325112867385, 1.000000000000000000, 0.9238795325112867385, 1.000000000000000000, 0.9238795325112848511, 1.000000000000001998 ) ) 
 REPRESENTATION_ITEM ( '' )  );
#7425 = CARTESIAN_POINT ( 'NONE',  ( -0.08325293014416509929, -0.4931997757357155510, 0.4003306813560889577 ) ) ;
#7426 = EDGE_CURVE ( 'NONE', #20410, #19381, #7118, .T. ) ;
#7427 = ADVANCED_FACE ( 'NONE', ( #12744 ), #13838, .T. ) ;
#7428 = CARTESIAN_POINT ( 'NONE',  ( 0.3107331597152522829, 4.640251624014341658, 0.02937061414036503879 ) ) ;
#7429 = AXIS2_PLACEMENT_3D ( 'NONE', #8023, #22900, #11952 ) ;
#7430 = CARTESIAN_POINT ( 'NONE',  ( 0.1144950937579611444, 0.2764156081756483641, 0.2376388888888919526 ) ) ;
#7431 = AXIS2_PLACEMENT_3D ( 'NONE', #10231, #15476, #4487 ) ;
#7432 = DIRECTION ( 'NONE',  ( 0.4999999999999992784, -0.8660254037844390407, 0.000000000000000000 ) ) ;
#7433 = CARTESIAN_POINT ( 'NONE',  ( -0.2923287055106771337, 0.1830357141881718552, -0.2123892367102620804 ) ) ;
#7434 = CARTESIAN_POINT ( 'NONE',  ( 0.2819296736111110424, 0.2541666665908000056, 0.1167790944451424923 ) ) ;
#7435 = DIRECTION ( 'NONE',  ( -0.000000000000000000, 1.000000000000000000, -0.000000000000000000 ) ) ;
#7436 = DIRECTION ( 'NONE',  ( -0.000000000000000000, -1.000000000000000000, -0.000000000000000000 ) ) ;
#7437 = CARTESIAN_POINT ( 'NONE',  ( -3.385114897866767815E-17, -0.2764156081756484196, -0.001944444444443294917 ) ) ;
#7438 = ORIENTED_EDGE ( 'NONE', *, *, #3928, .F. ) ;
#7439 = CARTESIAN_POINT ( 'NONE',  ( -0.2789096574489232094, 5.101491767903201691, -0.1383920302399104796 ) ) ;
#7440 = CARTESIAN_POINT ( 'NONE',  ( 0.4687500000000003886, -0.04437455914722442107, 0.4289794960421708381 ) ) ;
#7441 = CARTESIAN_POINT ( 'NONE',  ( 0.2819296736111110424, 0.5944444443685777957, -0.1167790944451423119 ) ) ;
#7442 = CARTESIAN_POINT ( 'NONE',  ( -0.3119999999999999996, 5.158416666666665762, -0.1292346314604056468 ) ) ;
#7443 = CARTESIAN_POINT ( 'NONE',  ( -0.1116596296178200276, 0.2044642856167432909, 0.3436530038418508792 ) ) ;
#7444 = CARTESIAN_POINT ( 'NONE',  ( -0.2819296736111110979, 4.422305555631421470, 0.000000000000000000 ) ) ;
#7445 = DIRECTION ( 'NONE',  ( 1.000000000000000000, 1.493785812010397745E-17, 1.707404996040164512E-16 ) ) ;
#7446 = CIRCLE ( 'NONE', #12914, 0.7500000000000001110 ) ;
#7447 = ORIENTED_EDGE ( 'NONE', *, *, #9157, .F. ) ;
#7448 = DIRECTION ( 'NONE',  ( 1.224646799147353207E-16, 0.000000000000000000, -1.000000000000000000 ) ) ;
#7449 = CARTESIAN_POINT ( 'NONE',  ( 5.178964085587577574E-17, 5.033416666742532186, 0.2819296736111110979 ) ) ;
#7450 = CARTESIAN_POINT ( 'NONE',  ( -0.2909262194017099845, 5.157387803290264472, 0.07538336336425460749 ) ) ;
#7451 = CARTESIAN_POINT ( 'NONE',  ( -0.3119999999999999996, 0.2124999999999996336, -3.820898013339742174E-17 ) ) ;
#7452 = CARTESIAN_POINT ( 'NONE',  ( 5.178964085587577574E-17, 4.755638888964754507, 0.2819296736111110979 ) ) ;
#7453 = PERSON_AND_ORGANIZATION ( #16982, #194 ) ;
#7454 = CARTESIAN_POINT ( 'NONE',  ( -0.09554088032208432613, 4.068872337771485270, 0.2980384827267206216 ) ) ;
#7455 = CARTESIAN_POINT ( 'NONE',  ( 0.2206173157302028787, 4.904944444444443441, 0.2206173157302027954 ) ) ;
#7456 = CARTESIAN_POINT ( 'NONE',  ( -0.1993543840281267465, 0.4729166665907999501, 0.1993543840281266633 ) ) ;
#7457 = ORIENTED_EDGE ( 'NONE', *, *, #5933, .T. ) ;
#7458 = ORIENTED_EDGE ( 'NONE', *, *, #7465, .F. ) ;
#7459 = CARTESIAN_POINT ( 'NONE',  ( -0.1993543840281267465, 0.1395833332574666907, 0.1993543840281266633 ) ) ;
#7460 = DIRECTION ( 'NONE',  ( 0.000000000000000000, 0.000000000000000000, 1.000000000000000000 ) ) ;
#7461 = FACE_OUTER_BOUND ( 'NONE', #7930, .T. ) ;
#7462 = CARTESIAN_POINT ( 'NONE',  ( 0.1236067977499789861, 0.2714285714285713524, -0.3804226065180614236 ) ) ;
#7463 = CARTESIAN_POINT ( 'NONE',  ( -0.1306872919485614903, 0.3155070326520293400, -0.05923611111111061478 ) ) ;
#7464 = CARTESIAN_POINT ( 'NONE',  ( -0.1294417382415922746, -0.3125000000000000000, 0.02236111111111264288 ) ) ;
#7465 = EDGE_CURVE ( 'NONE', #14874, #9859, #21669, .T. ) ;
#7466 = CARTESIAN_POINT ( 'NONE',  ( -0.2565929520051963841, 3.885670105107792427, -0.1774938258202259367 ) ) ;
#7467 = CARTESIAN_POINT ( 'NONE',  ( 0.1993543840281266355, 0.2506944443685777957, 0.1993543840281267465 ) ) ;
#7468 = DIRECTION ( 'NONE',  ( 0.000000000000000000, 0.000000000000000000, -1.000000000000000000 ) ) ;
#7469 = CARTESIAN_POINT ( 'NONE',  ( -0.2819296736111110424, 4.536888888964754507, 0.1167790944451424923 ) ) ;
#7470 = CARTESIAN_POINT ( 'NONE',  ( 0.1236067977499789028, 0.01964285694777236080, 0.3804226065180614791 ) ) ;
#7471 = CARTESIAN_POINT ( 'NONE',  ( -0.2815565333327582631, -9.420544349976224069E-18, -0.2815901784494979077 ) ) ;
#7472 = EDGE_CURVE ( 'NONE', #20446, #7699, #4260, .T. ) ;
#7473 = CARTESIAN_POINT ( 'NONE',  ( 0.1167790944451422702, 5.182722222298088433, -0.2819296736111110424 ) ) ;
#7474 = CARTESIAN_POINT ( 'NONE',  ( -0.1993543840281266910, 4.457027777853642903, -0.1993543840281266910 ) ) ;
#7475 = CARTESIAN_POINT ( 'NONE',  ( 0.004295427132208190675, 3.765940144888689556, -0.3119999790882598822 ) ) ;
#7476 = DIRECTION ( 'NONE',  ( 0.000000000000000000, 0.000000000000000000, 1.000000000000000000 ) ) ;
#7477 = CC_DESIGN_PERSON_AND_ORGANIZATION_ASSIGNMENT ( #12363, #21488, ( #19837 ) ) ;
#7478 = CARTESIAN_POINT ( 'NONE',  ( -0.3119999999999998885, 4.116750000151731648, 0.1292346314604058410 ) ) ;
#7479 = EDGE_CURVE ( 'NONE', #4265, #10744, #21904, .T. ) ;
#7480 = CARTESIAN_POINT ( 'NONE',  ( -0.2819296736111110979, 4.588972222298088433, 0.000000000000000000 ) ) ;
#7481 = CARTESIAN_POINT ( 'NONE',  ( 0.1015006192750689817, 3.724843167714382286, -0.2819296736111111534 ) ) ;
#7482 = CARTESIAN_POINT ( 'NONE',  ( -0.1567390680356932908, -0.2674066423995976605, -0.09867016728294440708 ) ) ;
#7483 = ORIENTED_EDGE ( 'NONE', *, *, #23504, .F. ) ;
#7484 = ORIENTED_EDGE ( 'NONE', *, *, #13192, .F. ) ;
#7485 = PERSON_AND_ORGANIZATION_ROLE ( 'design_supplier' ) ;
#7486 = CARTESIAN_POINT ( 'NONE',  ( -0.2918969027557561380, -0.06668494381005772575, 0.4106116311576339384 ) ) ;
#7487 = CARTESIAN_POINT ( 'NONE',  ( 0.2676934969451048585, -0.3758505236666522253, 0.4334994210334167652 ) ) ;
#7488 = FACE_OUTER_BOUND ( 'NONE', #6763, .T. ) ;
#7489 = ORIENTED_EDGE ( 'NONE', *, *, #11572, .T. ) ;
#7490 = CARTESIAN_POINT ( 'NONE',  ( -0.2206173157302028787, 0.4347222220704892726, 0.2206173157302027954 ) ) ;
#7491 = VERTEX_POINT ( 'NONE', #8733 ) ;
#7492 = CARTESIAN_POINT ( 'NONE',  ( 0.3124999999999993339, -0.1294417382415928852, 0.2029166666666696039 ) ) ;
#7493 = CARTESIAN_POINT ( 'NONE',  ( -0.2711786023059446493, 3.719745625394835109, -0.1610394760142928317 ) ) ;
#7494 = CARTESIAN_POINT ( 'NONE',  ( 2.326421213736078119E-17, 0.1544642856167433020, -0.3799334167787516425 ) ) ;
#7495 = CARTESIAN_POINT ( 'NONE',  ( 0.1572698204966380964, 3.983617205690540786, -0.2725461618487980409 ) ) ;
#7496 = VERTEX_POINT ( 'NONE', #22025 ) ;
#7497 = ADVANCED_FACE ( 'NONE', ( #10465 ), #17894, .T. ) ;
#7498 = CARTESIAN_POINT ( 'NONE',  ( -0.2233192592356399442, 0.1794642856167432687, -0.3073725909049499494 ) ) ;
#7499 = CARTESIAN_POINT ( 'NONE',  ( 0.1675087228796504069, 5.076665303775934390, 0.2633721787117046520 ) ) ;
#7500 = CARTESIAN_POINT ( 'NONE',  ( 0.000000000000000000, 0.2764156081756484196, 0.1855555555555581937 ) ) ;
#7501 = EDGE_CURVE ( 'NONE', #19685, #21037, #4240, .T. ) ;
#7502 = CARTESIAN_POINT ( 'NONE',  ( 0.1993543840281266633, 4.332027777853642903, -0.1993543840281266910 ) ) ;
#7503 = CARTESIAN_POINT ( 'NONE',  ( -0.2819296736111110424, 5.134111111186975940, 0.1167790944451424923 ) ) ;
#7504 = CARTESIAN_POINT ( 'NONE',  ( 0.1762772571227061713, -0.2274112121558803656, 0.3992673050735688900 ) ) ;
#7505 = CARTESIAN_POINT ( 'NONE',  ( -0.4620259694561524855, 0.2880908832651556950, 0.04413116910601659615 ) ) ;
#7506 = CARTESIAN_POINT ( 'NONE',  ( -0.3119999999999999996, 3.884111111111110404, 0.000000000000000000 ) ) ;
#7507 = CARTESIAN_POINT ( 'NONE',  ( -0.2206173157302027676, 4.786888889040620931, 0.2206173157302028787 ) ) ;
#7508 = AXIS2_PLACEMENT_3D ( 'NONE', #3875, #5701, #213 ) ;
#7509 = EDGE_CURVE ( 'NONE', #23140, #5916, #7364, .T. ) ;
#7510 = CARTESIAN_POINT ( 'NONE',  ( -0.2819296736111110424, 5.203332556872311443, 0.1092791156175831058 ) ) ;
#7511 = CARTESIAN_POINT ( 'NONE',  ( -0.5116234456863466562, 0.9548081934128058723, 2.549370209580444246 ) ) ;
#7512 = CARTESIAN_POINT ( 'NONE',  ( -0.2233192592356399442, 0.1616071427596004473, -0.3073725909049499494 ) ) ;
#7513 = CARTESIAN_POINT ( 'NONE',  ( 0.3950000000000000178, 2.665000000000000036, -1.966000000000000192 ) ) ;
#7514 = APPROVAL_STATUS ( 'not_yet_approved' ) ;
#7515 = CARTESIAN_POINT ( 'NONE',  ( 9.101228903679513089E-16, 0.3732142855192008835, 0.4000000000000000222 ) ) ;
#7516 = CARTESIAN_POINT ( 'NONE',  ( -0.1167790944451423257, 5.064666666742533074, -0.2819296736111110424 ) ) ;
#7517 = CARTESIAN_POINT ( 'NONE',  ( 0.1167790944451424506, 3.939666666742532186, 0.2819296736111110424 ) ) ;
#7518 = VECTOR ( 'NONE', #13586, 39.37007874015748143 ) ;
#7519 = CARTESIAN_POINT ( 'NONE',  ( 0.2491691211422967234, -0.3865828334249452047, 0.4343841983240312454 ) ) ;
#7520 = CARTESIAN_POINT ( 'NONE',  ( 0.000000000000000000, 0.000000000000000000, 1.326383476483184332 ) ) ;
#7521 = ADVANCED_FACE ( 'NONE', ( #12187 ), #16471, .T. ) ;
#7522 = EDGE_CURVE ( 'NONE', #3235, #20411, #22044, .T. ) ;
#7523 = CARTESIAN_POINT ( 'NONE',  ( 0.2764156081756483641, 0.1144950937579610195, 0.1195833333333354703 ) ) ;
#7524 = CARTESIAN_POINT ( 'NONE',  ( -0.2819296736111110979, 0.1847222221463555858, -0.1167790944451423396 ) ) ;
#7525 = CARTESIAN_POINT ( 'NONE',  ( -0.1954553509668046640, 0.1954553509668046918, 0.3105555555555591929 ) ) ;
#7526 = CARTESIAN_POINT ( 'NONE',  ( -0.1167790944451423535, 4.877166666742533963, 0.2819296736111110424 ) ) ;
#7527 = CARTESIAN_POINT ( 'NONE',  ( -0.1993543840281266910, 4.957027777853642903, -0.1993543840281266910 ) ) ;
#7528 = DIRECTION ( 'NONE',  ( -0.000000000000000000, 1.000000000000000000, -0.000000000000000000 ) ) ;
#7529 = CARTESIAN_POINT ( 'NONE',  ( -0.5116234456863258950, 1.041821957232212270, -2.640781157734871876 ) ) ;
#7530 = CARTESIAN_POINT ( 'NONE',  ( -1.910449006669871087E-17, 4.592444444444443441, -0.3119999999999999996 ) ) ;
#7531 = CARTESIAN_POINT ( 'NONE',  ( 0.000000000000000000, 5.384999999999999787, 0.000000000000000000 ) ) ;
#7532 = CARTESIAN_POINT ( 'NONE',  ( 0.1292346314604056190, 4.588972222222221120, -0.3119999999999999996 ) ) ;
#7533 = CARTESIAN_POINT ( 'NONE',  ( 0.2819296736111110979, 3.769527777853642903, -3.452642723725051716E-17 ) ) ;
#7534 = CARTESIAN_POINT ( 'NONE',  ( 0.8119709581221709049, 2.978485840173427324, -1.588368860739399313 ) ) ;
#7535 = EDGE_CURVE ( 'NONE', #9500, #23062, #3512, .T. ) ;
#7536 = CARTESIAN_POINT ( 'NONE',  ( 7.484242640931070629E-07, 4.016084960865516251, 0.3119999999981048489 ) ) ;
#7537 = DIRECTION ( 'NONE',  ( -0.8246458398455801531, 0.5656493956731305506, 0.000000000000000000 ) ) ;
#7538 = DIRECTION ( 'NONE',  ( -0.000000000000000000, -0.000000000000000000, 1.000000000000000000 ) ) ;
#7539 = VERTEX_POINT ( 'NONE', #19978 ) ;
#7540 = VECTOR ( 'NONE', #22928, 39.37007874015747433 ) ;
#7541 = CARTESIAN_POINT ( 'NONE',  ( -0.03772805809618737238, 4.100482206091769832, -0.3120000000000012208 ) ) ;
#7542 = DIRECTION ( 'NONE',  ( -0.000000000000000000, -1.000000000000000000, -0.000000000000000000 ) ) ;
#7543 = CARTESIAN_POINT ( 'NONE',  ( -0.1144950937579609779, 0.2764156081756484196, 0.3001388888888924522 ) ) ;
#7544 = CARTESIAN_POINT ( 'NONE',  ( 3.820898013339742174E-17, 5.384999999999999787, 0.3119999999999999996 ) ) ;
#7545 = CARTESIAN_POINT ( 'NONE',  ( 3.820898013339742174E-17, 5.384999999999999787, 0.3119999999999999996 ) ) ;
#7546 = ORIENTED_EDGE ( 'NONE', *, *, #4095, .F. ) ;
#7547 = CARTESIAN_POINT ( 'NONE',  ( 0.1116596296178199860, 0.3830357141881718386, -0.3436530038418508792 ) ) ;
#7548 = CARTESIAN_POINT ( 'NONE',  ( 0.1167790944451423535, 0.3027777777019111105, 0.2819296736111110424 ) ) ;
#7549 = CARTESIAN_POINT ( 'NONE',  ( 1.910449006669871087E-17, 0.1916666665149337478, -0.3119999999999999996 ) ) ;
#7550 = CARTESIAN_POINT ( 'NONE',  ( 2.100416254512341485, 2.978485840173427324, -2.201288568297000925 ) ) ;
#7551 = FACE_OUTER_BOUND ( 'NONE', #11421, .T. ) ;
#7552 = CARTESIAN_POINT ( 'NONE',  ( -0.1954553509668046640, 0.1954553509668046918, 0.03277777777777921009 ) ) ;
#7553 = VECTOR ( 'NONE', #5028, 39.37007874015748143 ) ;
#7554 = ORIENTED_EDGE ( 'NONE', *, *, #3784, .T. ) ;
#7555 = CARTESIAN_POINT ( 'NONE',  ( 0.000000000000000000, 0.000000000000000000, 0.2500000000000000000 ) ) ;
#7556 = DIRECTION ( 'NONE',  ( 0.000000000000000000, 0.000000000000000000, -1.000000000000000000 ) ) ;
#7557 = CARTESIAN_POINT ( 'NONE',  ( 0.3119999999999999996, -0.03402777777777810791, -0.1292346314604056468 ) ) ;
#7558 = CARTESIAN_POINT ( 'NONE',  ( -0.3119999999999999996, 5.269527777777777366, -0.1292346314604056468 ) ) ;
#7559 = CARTESIAN_POINT ( 'NONE',  ( 0.2923287055106771337, 0.1473214284738861568, 0.2123892367102621359 ) ) ;
#7560 = VERTEX_POINT ( 'NONE', #23988 ) ;
#7561 = CARTESIAN_POINT ( 'NONE',  ( -0.2819296736111110424, 4.203555555631421470, 0.1167790944451424923 ) ) ;
#7562 = EDGE_CURVE ( 'NONE', #18493, #13675, #7300, .T. ) ;
#7563 = CARTESIAN_POINT ( 'NONE',  ( 1.573500000000000343, -3.414809992080329023E-17, -1.412500000000000089 ) ) ;
#7564 = CARTESIAN_POINT ( 'NONE',  ( 0.3600616651536501234, -9.204707668395288817E-18, -0.03256283952987127500 ) ) ;
#7565 = ORIENTED_EDGE ( 'NONE', *, *, #9690, .F. ) ;
#7566 = VERTEX_POINT ( 'NONE', #20341 ) ;
#7567 = CARTESIAN_POINT ( 'NONE',  ( -5.731347020009612645E-17, 0.3374999999999996336, 0.3119999999999999996 ) ) ;
#7568 = CARTESIAN_POINT ( 'NONE',  ( 0.1993543840281266633, 4.998694444520309865, -0.1993543840281266910 ) ) ;
#7569 = LINE ( 'NONE', #11237, #11894 ) ;
#7570 = AXIS2_PLACEMENT_3D ( 'NONE', #8266, #11827, #11589 ) ;
#7571 = CARTESIAN_POINT ( 'NONE',  ( 7.772715683692237754, 4.627125918905005797, -2.990953229846804451 ) ) ;
#7572 = CARTESIAN_POINT ( 'NONE',  ( 0.000000000000000000, 3.659999999999999698, 0.000000000000000000 ) ) ;
#7573 = CARTESIAN_POINT ( 'NONE',  ( 0.06335377612981404893, 0.2017409185161840035, -0.4000000000000001887 ) ) ;
#7574 = CARTESIAN_POINT ( 'NONE',  ( 0.1993543840281266633, 4.720916666742532186, -0.1993543840281266910 ) ) ;
#7575 = ITEM_DEFINED_TRANSFORMATION ( 'NONE', 'NONE', #23538,  #9127 ) ;
#7576 = DIRECTION ( 'NONE',  ( 0.5000000000000003331, 0.000000000000000000, 0.8660254037844383745 ) ) ;
#7577 = CARTESIAN_POINT ( 'NONE',  ( 2.936000000000001720, 2.740000000000000213, -0.05000000000000028727 ) ) ;
#7578 = CARTESIAN_POINT ( 'NONE',  ( 0.2819296736111110424, 0.4347222221463555858, 0.1167790944451424923 ) ) ;
#7579 = VERTEX_POINT ( 'NONE', #3629 ) ;
#7580 = CARTESIAN_POINT ( 'NONE',  ( -5.178964085587577574E-17, 0.3131944443685777957, 0.2819296736111110979 ) ) ;
#7581 = DIRECTION ( 'NONE',  ( -1.224646799147350495E-16, 0.000000000000000000, -1.000000000000000000 ) ) ;
#7582 = DIRECTION ( 'NONE',  ( 0.000000000000000000, 0.000000000000000000, -1.000000000000000000 ) ) ;
#7583 = CARTESIAN_POINT ( 'NONE',  ( 2.575339694675500462E-17, 0.1321428571428571175, -0.4205848896953069405 ) ) ;
#7584 = DIRECTION ( 'NONE',  ( -0.000000000000000000, -1.000000000000000000, -0.000000000000000000 ) ) ;
#7585 = CARTESIAN_POINT ( 'NONE',  ( -0.04811092099938358430, -0.5134890241753798934, 0.05816431335569525324 ) ) ;
#7586 = LINE ( 'NONE', #15037, #15969 ) ;
#7587 = CARTESIAN_POINT ( 'NONE',  ( 0.1993543840281266355, 0.1951388888130222155, 0.1993543840281267465 ) ) ;
#7588 = CARTESIAN_POINT ( 'NONE',  ( -0.1167790944451422702, 0.05277777770191114520, -0.2819296736111110424 ) ) ;
#7589 = CARTESIAN_POINT ( 'NONE',  ( -0.1993543840281266910, 4.248694444520310753, -0.1993543840281266910 ) ) ;
#7590 = CARTESIAN_POINT ( 'NONE',  ( 2.575339694675500462E-17, -0.01964285733794191718, -0.4205848896953069405 ) ) ;
#7591 = CIRCLE ( 'NONE', #22379, 0.3308333333333332571 ) ;
#7592 = CARTESIAN_POINT ( 'NONE',  ( -0.1993543840281266355, 4.762583333409199149, 0.1993543840281267465 ) ) ;
#7593 = ADVANCED_FACE ( 'NONE', ( #11080 ), #14252, .F. ) ;
#7594 = CARTESIAN_POINT ( 'NONE',  ( -0.2819296736111110979, 4.516055555631421470, -0.1167790944451422980 ) ) ;
#7595 = CARTESIAN_POINT ( 'NONE',  ( 0.000000000000000000, 5.384999999999999787, -0.3119999999999999996 ) ) ;
#7596 = CARTESIAN_POINT ( 'NONE',  ( 0.2748323731540602832, 3.923346161548030953, -0.1544819192003367703 ) ) ;
#7597 = CARTESIAN_POINT ( 'NONE',  ( 0.2206173157302028787, 4.134111111262843252, 0.2206173157302027954 ) ) ;
#7598 = PRODUCT_DEFINITION_FORMATION_WITH_SPECIFIED_SOURCE ( 'ANY', '', #19646, .NOT_KNOWN. ) ;
#7599 = LINE ( 'NONE', #22348, #12660 ) ;
#7600 = CARTESIAN_POINT ( 'NONE',  ( 0.3125000000000000000, 3.827021247335477694E-17, 1.326383476483184332 ) ) ;
#7601 = ORIENTED_EDGE ( 'NONE', *, *, #12651, .T. ) ;
#7602 = VERTEX_POINT ( 'NONE', #10599 ) ;
#7603 = PERSON_AND_ORGANIZATION ( #15518, #2538 ) ;
#7604 = CARTESIAN_POINT ( 'NONE',  ( -0.1898046044842733593, -0.2363956207630708017, 0.4143648991452117958 ) ) ;
#7605 = CARTESIAN_POINT ( 'NONE',  ( -0.2471927412204658892, 4.841317424427891147, 0.1938822679348655431 ) ) ;
#7606 = DIRECTION ( 'NONE',  ( 0.000000000000000000, 1.000000000000000000, 0.000000000000000000 ) ) ;
#7607 = EDGE_LOOP ( 'NONE', ( #17840, #2972, #5167, #7864 ) ) ;
#7608 = CARTESIAN_POINT ( 'NONE',  ( -5.731347020009612645E-17, 0.4972222220704892726, 0.3119999999999999996 ) ) ;
#7609 = ORIENTED_EDGE ( 'NONE', *, *, #17461, .F. ) ;
#7610 = LINE ( 'NONE', #7259, #3945 ) ;
#7611 = CARTESIAN_POINT ( 'NONE',  ( 0.06860513764972499262, 4.740183546148049487, 0.3064380078074160352 ) ) ;
#7612 = CARTESIAN_POINT ( 'NONE',  ( -0.1116596296178199582, 0.1580357141881718608, -0.3436530038418508792 ) ) ;
#7613 = LINE ( 'NONE', #22487, #5002 ) ;
#7614 = VERTEX_POINT ( 'NONE', #18027 ) ;
#7615 = APPROVAL_PERSON_ORGANIZATION ( #18461, #14170, #14699 ) ;
#7616 = CARTESIAN_POINT ( 'NONE',  ( -0.3613381517857143232, 0.1151785713310289894, -0.1174058825155741143 ) ) ;
#7617 = ORIENTED_EDGE ( 'NONE', *, *, #14815, .F. ) ;
#7618 = DIRECTION ( 'NONE',  ( 1.000000000000000000, 0.000000000000000000, 0.000000000000000000 ) ) ;
#7619 = CARTESIAN_POINT ( 'NONE',  ( -0.3032940676781117340, 4.666745353835117349, -0.07416804978120151992 ) ) ;
#7620 = CARTESIAN_POINT ( 'NONE',  ( 5.178964085587577574E-17, 4.200083333409199149, 0.2819296736111110979 ) ) ;
#7621 = CARTESIAN_POINT ( 'NONE',  ( -0.2681267372834953977, -0.3756399061183363086, 0.4344383781808794365 ) ) ;
#7622 = DIRECTION ( 'NONE',  ( 0.000000000000000000, -1.000000000000000000, 0.000000000000000000 ) ) ;
#7623 = CARTESIAN_POINT ( 'NONE',  ( -0.2206173157302027676, 3.835499999999998799, 0.2206173157302028787 ) ) ;
#7624 = CARTESIAN_POINT ( 'NONE',  ( -0.3119999999999998885, 4.727861111262843252, 0.1292346314604058410 ) ) ;
#7625 = AXIS2_PLACEMENT_3D ( 'NONE', #23401, #12224, #19634 ) ;
#7626 = CARTESIAN_POINT ( 'NONE',  ( -0.1167790944451423535, 5.154944444520309865, 0.2819296736111110979 ) ) ;
#7627 = CARTESIAN_POINT ( 'NONE',  ( -0.1993543840281266355, 4.193138888964754507, 0.1993543840281267465 ) ) ;
#7628 = CARTESIAN_POINT ( 'NONE',  ( -0.03429112345822225155, 3.903953541745516453, 0.3120000015083762568 ) ) ;
#7629 = ORIENTED_EDGE ( 'NONE', *, *, #16816, .F. ) ;
#7630 = CARTESIAN_POINT ( 'NONE',  ( 0.2233192592356400275, 0.1473214284738861568, -0.3073725909049499494 ) ) ;
#7631 = ORIENTED_EDGE ( 'NONE', *, *, #21398, .T. ) ;
#7632 = SECURITY_CLASSIFICATION ( '', '', #16490 ) ;
#7633 = CARTESIAN_POINT ( 'NONE',  ( -0.06818719739654979795, 0.05951326967753017838, 0.3015576727156116243 ) ) ;
#7634 = VERTEX_POINT ( 'NONE', #1325 ) ;
#7635 = EDGE_CURVE ( 'NONE', #5544, #7381, #21804, .T. ) ;
#7636 = PERSON_AND_ORGANIZATION ( #15518, #2538 ) ;
#7637 = CARTESIAN_POINT ( 'NONE',  ( 0.4641327083039680779, 0.2728248698625151403, 0.04698599556840849650 ) ) ;
#7638 = CARTESIAN_POINT ( 'NONE',  ( -0.1993543840281266355, 5.082027777853643791, 0.1993543840281267465 ) ) ;
#7639 = CARTESIAN_POINT ( 'NONE',  ( -0.2819296736111110979, 3.977861111186976828, 0.000000000000000000 ) ) ;
#7640 = VECTOR ( 'NONE', #13684, 39.37007874015748143 ) ;
#7641 = DIRECTION ( 'NONE',  ( 0.000000000000000000, -0.8660254037843519992, -0.5000000000001502132 ) ) ;
#7642 = EDGE_CURVE ( 'NONE', #6378, #1715, #726, .T. ) ;
#7643 = CARTESIAN_POINT ( 'NONE',  ( 0.2233192592356399164, 0.3401785713310290227, 0.3073725909049500604 ) ) ;
#7644 = CARTESIAN_POINT ( 'NONE',  ( -0.1144950937579609918, -0.2764156081756484196, 0.2654166666666700203 ) ) ;
#7645 = CARTESIAN_POINT ( 'NONE',  ( 0.1167790944451423535, 0.4277777777019111660, 0.2819296736111110979 ) ) ;
#7646 = CARTESIAN_POINT ( 'NONE',  ( -0.1954553509668046918, -0.1954553509668046640, 0.4355555555555601921 ) ) ;
#7647 = CARTESIAN_POINT ( 'NONE',  ( -0.2819296736111110424, 4.870222222298087544, 0.1167790944451424923 ) ) ;
#7648 = DIRECTION ( 'NONE',  ( -0.8660254037844434816, 0.000000000000000000, 0.4999999999999913403 ) ) ;
#7649 = CARTESIAN_POINT ( 'NONE',  ( 0.2819296736111110424, 4.884111111186975940, -0.1167790944451423396 ) ) ;
#7650 = DIRECTION ( 'NONE',  ( -0.5000000000000043299, 0.000000000000000000, 0.8660254037844362651 ) ) ;
#7651 = CARTESIAN_POINT ( 'NONE',  ( 0.2199754637977810179, 4.856310113992576838, 0.2213457067253412347 ) ) ;
#7652 = CARTESIAN_POINT ( 'NONE',  ( 0.3119999999999999996, 4.078555555555555046, -3.820898013339742174E-17 ) ) ;
#7653 = CARTESIAN_POINT ( 'NONE',  ( 0.4645343760433821023, 0.2721270390806222461, 0.05893285591566543163 ) ) ;
#7654 = CARTESIAN_POINT ( 'NONE',  ( -0.3119999999999999996, 4.547305555555555934, -0.1292346314604056468 ) ) ;
#7655 = CARTESIAN_POINT ( 'NONE',  ( -0.1167790944451423535, 3.752166666742532186, 0.2819296736111110979 ) ) ;
#7656 = CARTESIAN_POINT ( 'NONE',  ( 0.02997679058488651391, 4.987417349384497101, -0.3106133072238613235 ) ) ;
#7657 = CARTESIAN_POINT ( 'NONE',  ( -0.1052608686101951518, 3.735246098045301721, 0.2937075919364244281 ) ) ;
#7658 = CARTESIAN_POINT ( 'NONE',  ( 0.2916724325548126773, 4.582301768384474450, 0.1117771105708152413 ) ) ;
#7659 = ORIENTED_EDGE ( 'NONE', *, *, #23418, .T. ) ;
#7660 = CARTESIAN_POINT ( 'NONE',  ( -0.1791194818499489971, 4.104818640075733605, -0.2582428417481592020 ) ) ;
#7661 = EDGE_CURVE ( 'NONE', #21247, #3503, #11323, .T. ) ;
#7662 = CARTESIAN_POINT ( 'NONE',  ( 0.2856515860211834013, 4.644828526069876951, -0.1311504800872141663 ) ) ;
#7663 = CARTESIAN_POINT ( 'NONE',  ( -3.863846776457871776E-17, -0.3155070326520292845, -0.08701388888888821060 ) ) ;
#7664 = DIRECTION ( 'NONE',  ( 0.000000000000000000, 0.000000000000000000, -1.000000000000000000 ) ) ;
#7665 = EDGE_CURVE ( 'NONE', #10917, #1519, #16325, .T. ) ;
#7666 = CARTESIAN_POINT ( 'NONE',  ( 0.000000000000000000, 0.000000000000000000, 1.326383476483184332 ) ) ;
#7667 = VERTEX_POINT ( 'NONE', #24108 ) ;
#7668 = CARTESIAN_POINT ( 'NONE',  ( -0.1116596296178200276, 0.2758928570453147433, 0.3436530038418508792 ) ) ;
#7669 = CIRCLE ( 'NONE', #16245, 0.2495000000000007212 ) ;
#7670 = CARTESIAN_POINT ( 'NONE',  ( 0.2819296736111110979, 0.4798611110352444808, 0.000000000000000000 ) ) ;
#7671 = CARTESIAN_POINT ( 'NONE',  ( 0.4687500000000002776, -0.2598076211353317344, 0.06112444011295377344 ) ) ;
#7672 = CARTESIAN_POINT ( 'NONE',  ( 0.1668575117781267991, 0.2231724005212394890, -1.220106870630045748 ) ) ;
#7673 = CARTESIAN_POINT ( 'NONE',  ( 0.2730703793714973626, 0.3836086203274273188, 0.4181140142936810578 ) ) ;
#7674 = CARTESIAN_POINT ( 'NONE',  ( -3.385114897866767815E-17, -0.2764156081756484196, 0.1647222222222247123 ) ) ;
#7675 = CARTESIAN_POINT ( 'NONE',  ( -0.3062927780948892509, 5.103999883774990920, -0.05168569905423461147 ) ) ;
#7676 = CARTESIAN_POINT ( 'NONE',  ( 0.4592090122005416108, 0.09026097205167347981, 0.4297114009649623534 ) ) ;
#7677 = CARTESIAN_POINT ( 'NONE',  ( -0.1292346314604058410, 0.3340277777777773682, 0.3119999999999998885 ) ) ;
#7678 = CARTESIAN_POINT ( 'NONE',  ( -0.3119999999999999996, 5.161888888888888083, 0.000000000000000000 ) ) ;
#7679 = CARTESIAN_POINT ( 'NONE',  ( -0.2819296736111110979, 4.255638888964754507, 0.000000000000000000 ) ) ;
#7680 = DIRECTION ( 'NONE',  ( 0.000000000000000000, 0.000000000000000000, -1.000000000000000000 ) ) ;
#7681 = EDGE_CURVE ( 'NONE', #10527, #18852, #5941, .T. ) ;
#7682 = FACE_OUTER_BOUND ( 'NONE', #5043, .T. ) ;
#7683 = EDGE_LOOP ( 'NONE', ( #17423, #21637, #14080, #16129 ) ) ;
#7684 = CARTESIAN_POINT ( 'NONE',  ( -0.4620259694561524855, -0.2880908832651560281, 0.04413116910601651982 ) ) ;
#7685 = CARTESIAN_POINT ( 'NONE',  ( -0.1993543840281266355, 4.915361111186976828, 0.1993543840281267465 ) ) ;
#7686 = EDGE_CURVE ( 'NONE', #20226, #397, #19323, .T. ) ;
#7687 = CARTESIAN_POINT ( 'NONE',  ( -0.1833914370424524765, 5.148434169276817407, -0.2416754135350870913 ) ) ;
#7688 = EDGE_CURVE ( 'NONE', #22655, #17146, #3993, .T. ) ;
#7689 = AXIS2_PLACEMENT_3D ( 'NONE', #14435, #23313, #16385 ) ;
#7690 = LENGTH_MEASURE_WITH_UNIT ( LENGTH_MEASURE( 0.02539999999999999897 ), #11358 );
#7691 = CARTESIAN_POINT ( 'NONE',  ( 0.000000000000000000, 3.738758431839877614E-19, 0.004799741732707325965 ) ) ;
#7692 = CARTESIAN_POINT ( 'NONE',  ( -1.910449006669871087E-17, 3.981333333333332725, -0.3119999999999999996 ) ) ;
#7693 = B_SPLINE_CURVE_WITH_KNOTS ( 'NONE', 3,
 ( #22319, #2215, #2082, #17081, #11603, #490 ),
 .UNSPECIFIED., .F., .F.,
 ( 4, 2, 4 ),
 ( 0.006549771812455102565, 0.009815615986340283511, 0.01308146016022546446 ),
 .UNSPECIFIED. ) ;
#7694 = CARTESIAN_POINT ( 'NONE',  ( 5.178964085587577574E-17, 4.588972222298087544, 0.2819296736111110979 ) ) ;
#7695 = ADVANCED_FACE ( 'NONE', ( #15662 ), #5820, .T. ) ;
#7696 = CARTESIAN_POINT ( 'NONE',  ( -0.008323108056630971682, 4.044058012889800935, -0.3119051118721674065 ) ) ;
#7697 = CARTESIAN_POINT ( 'NONE',  ( -0.1954553509668046640, 0.1954553509668046918, 0.03277777777777921009 ) ) ;
#7698 = CARTESIAN_POINT ( 'NONE',  ( 0.1993543840281266355, 0.5979166665908001166, 0.1993543840281267465 ) ) ;
#7699 = VERTEX_POINT ( 'NONE', #9488 ) ;
#7700 = CARTESIAN_POINT ( 'NONE',  ( 0.1167790944451423535, 0.2611111110352444808, 0.2819296736111110424 ) ) ;
#7701 = CARTESIAN_POINT ( 'NONE',  ( 2.100109879709019189, 2.740000000000000213, -3.013126998327187778 ) ) ;
#7702 = CARTESIAN_POINT ( 'NONE',  ( -0.3125000000000000555, 1.913510623667739771E-17, 0.1716666666666689933 ) ) ;
#7703 = CARTESIAN_POINT ( 'NONE',  ( -7.726019084026502927E-17, 0.09642857142857139130, 0.4205848896953069405 ) ) ;
#7704 = CARTESIAN_POINT ( 'NONE',  ( -0.1306872919485615459, -0.3155070326520293400, 0.07270833333333487358 ) ) ;
#7705 = CARTESIAN_POINT ( 'NONE',  ( -0.04626190099492148711, -0.5145565563726327563, 0.07046568677121804736 ) ) ;
#7706 = CARTESIAN_POINT ( 'NONE',  ( 0.7847114317029997288, 0.000000000000000000, -0.6249999999999962252 ) ) ;
#7707 = CARTESIAN_POINT ( 'NONE',  ( 0.1167790944451423119, 0.2124999999241334037, -0.2819296736111110979 ) ) ;
#7708 = CARTESIAN_POINT ( 'NONE',  ( 0.1993543840281266355, 0.3062499999241333759, 0.1993543840281267465 ) ) ;
#7709 = CARTESIAN_POINT ( 'NONE',  ( -0.1167790944451423257, 4.300777777853642903, -0.2819296736111110424 ) ) ;
#7710 = VECTOR ( 'NONE', #17639, 39.37007874015747433 ) ;
#7711 = CARTESIAN_POINT ( 'NONE',  ( 0.3236067977499789694, 0.1696428569477723136, 0.2351141009169893659 ) ) ;
#7712 = CARTESIAN_POINT ( 'NONE',  ( -0.2819296736111110424, 4.981333333409199149, 0.1167790944451424923 ) ) ;
#7713 = CARTESIAN_POINT ( 'NONE',  ( -0.1167790944451423119, 4.342444444520310753, -0.2819296736111110979 ) ) ;
#7714 = CARTESIAN_POINT ( 'NONE',  ( 0.2530624153226711526, 5.072996518863750026, 0.1824922298374807572 ) ) ;
#7715 = CARTESIAN_POINT ( 'NONE',  ( 0.3119999999999999996, 4.526472222222221120, -0.1292346314604056745 ) ) ;
#7716 = CARTESIAN_POINT ( 'NONE',  ( 0.2206173157302027954, 4.036888889040620931, -0.2206173157302028232 ) ) ;
#7717 = CARTESIAN_POINT ( 'NONE',  ( 0.1292346314604056745, 0.1395833333333330317, -0.3119999999999999996 ) ) ;
#7718 = CARTESIAN_POINT ( 'NONE',  ( -0.2351701443100413791, -0.2046330205465220486, -0.1004527702155444124 ) ) ;
#7719 = ORIENTED_EDGE ( 'NONE', *, *, #19953, .F. ) ;
#7720 = AXIS2_PLACEMENT_3D ( 'NONE', #7989, #4451, #7870 ) ;
#7721 = ADVANCED_FACE ( 'NONE', ( #2177 ), #16327, .F. ) ;
#7722 = PERSON_AND_ORGANIZATION ( #15518, #2538 ) ;
#7723 = CARTESIAN_POINT ( 'NONE',  ( 0.1797085267211815662, 3.721720965436318362, -0.2172307213220433242 ) ) ;
#7724 = CARTESIAN_POINT ( 'NONE',  ( 0.3257020783361852523, -0.3421021315173797817, 0.4271664148355318047 ) ) ;
#7725 = CARTESIAN_POINT ( 'NONE',  ( -0.1912963777039489444, 4.993992924180794546, -0.2498290115581893456 ) ) ;
#7726 = ORIENTED_EDGE ( 'NONE', *, *, #21482, .F. ) ;
#7727 = CARTESIAN_POINT ( 'NONE',  ( -0.3119999999999999996, 0.5944444442927114824, -3.820898013339742174E-17 ) ) ;
#7728 = ORIENTED_EDGE ( 'NONE', *, *, #1230, .F. ) ;
#7729 = CYLINDRICAL_SURFACE ( 'NONE', #7011, 0.3125000000000000000 ) ;
#7730 = CARTESIAN_POINT ( 'NONE',  ( 0.4593750000000004219, 0.2760455974562900927, 0.3779506566538943235 ) ) ;
#7731 = CARTESIAN_POINT ( 'NONE',  ( 0.02974333840505747131, 4.765210078712510899, -0.3106355410811253437 ) ) ;
#7732 = CARTESIAN_POINT ( 'NONE',  ( -0.2233192592356399997, -0.03125000009754239083, 0.3073725909049499494 ) ) ;
#7733 = DIRECTION ( 'NONE',  ( 0.000000000000000000, -0.7071067811865464625, -0.7071067811865486830 ) ) ;
#7734 = ORIENTED_EDGE ( 'NONE', *, *, #2767, .T. ) ;
#7735 = CARTESIAN_POINT ( 'NONE',  ( 0.1116596296178199027, 0.1401785713310290393, 0.3436530038418508792 ) ) ;
#7736 = ORIENTED_EDGE ( 'NONE', *, *, #13075, .F. ) ;
#7737 = DIRECTION ( 'NONE',  ( -0.000000000000000000, 1.000000000000000000, -0.000000000000000000 ) ) ;
#7738 = DIRECTION ( 'NONE',  ( -1.000000000000000000, 0.000000000000000000, 0.000000000000000000 ) ) ;
#7739 = B_SPLINE_CURVE_WITH_KNOTS ( 'NONE', 3,
 ( #7505, #17583, #58, #7858, #20552, #3847, #15307, #23171, #15186, #13017 ),
 .UNSPECIFIED., .F., .F.,
 ( 4, 2, 2, 2, 4 ),
 ( 0.000000000000000000, 0.003270554913819859362, 0.006541109827639718724, 0.009811664741459578953, 0.01308221965527943745 ),
 .UNSPECIFIED. ) ;
#7740 = CARTESIAN_POINT ( 'NONE',  ( 0.2819296736111110979, 3.932722222298087544, 0.1167790944451422425 ) ) ;
#7741 = CARTESIAN_POINT ( 'NONE',  ( -0.2091198842963307158, -0.4097039017751712975, 0.4343513344076715410 ) ) ;
#7742 = CARTESIAN_POINT ( 'NONE',  ( 2.458533612140684792E-17, 0.1592944763917982509, -1.165725933896874400 ) ) ;
#7743 = CARTESIAN_POINT ( 'NONE',  ( -0.3119999999999999996, 3.772999999999999243, 0.000000000000000000 ) ) ;
#7744 = CIRCLE ( 'NONE', #14355, 0.2500000000000000000 ) ;
#7745 = CARTESIAN_POINT ( 'NONE',  ( 0.3119999999999999996, 4.752166666818398610, -3.820898013339742174E-17 ) ) ;
#7746 = CARTESIAN_POINT ( 'NONE',  ( 0.1993543840281267465, 4.887583333409199149, 0.1993543840281266633 ) ) ;
#7747 = ORIENTED_EDGE ( 'NONE', *, *, #21127, .T. ) ;
#7748 = CARTESIAN_POINT ( 'NONE',  ( -0.2819296736111110979, 4.297305555631420582, 0.000000000000000000 ) ) ;
#7749 = CARTESIAN_POINT ( 'NONE',  ( -0.3613381517857143788, 0.1044642856167432993, 0.1174058825155740310 ) ) ;
#7750 = CC_DESIGN_PERSON_AND_ORGANIZATION_ASSIGNMENT ( #17739, #8704, ( #11526 ) ) ;
#7751 = ORIENTED_EDGE ( 'NONE', *, *, #11438, .F. ) ;
#7752 = ORIENTED_EDGE ( 'NONE', *, *, #9178, .T. ) ;
#7753 = APPROVAL_DATE_TIME ( #315, #4769 ) ;
#7754 = B_SPLINE_CURVE_WITH_KNOTS ( 'NONE', 3,
 ( #772, #19790, #15533, #6739, #4784, #21138, #2612, #2838, #21380, #15774, #21495, #17480, #6502, #17966, #1256, #13952, #2725, #6617, #10179, #10297, #14183, #17602, #10056, #22956, #8204, #2965, #23072, #15653, #10421, #6258, #17720, #13718, #8445, #12139 ),
 .UNSPECIFIED., .F., .F.,
 ( 4, 2, 2, 2, 2, 2, 2, 2, 1, 1, 1, 1, 2, 2, 2, 2, 2, 2, 4 ),
 ( 0.7401386592960095268, 0.7424993613057664366, 0.7448600633155233464, 0.7472207653252802562, 0.7495814673350371660, 0.7507618183399156209, 0.7507802613243668155, 0.7507894828165924128, 0.7507987043088180101, 0.7508355902777205104, 0.7509093622155254000, 0.7510569060911351791, 0.7513519938423547373, 0.7519421693447939647, 0.7543028713545505415, 0.7554832223594288854, 0.7566635733643072292, 0.7578439243691855731, 0.7590242753740639170 ),
 .UNSPECIFIED. ) ;
#7755 = CARTESIAN_POINT ( 'NONE',  ( 0.4500000000000003442, -0.2598076211353317899, 0.3779506566538943235 ) ) ;
#7756 = CARTESIAN_POINT ( 'NONE',  ( 0.2819296736111110979, 5.213972222298088433, -3.452642723725051716E-17 ) ) ;
#7757 = CARTESIAN_POINT ( 'NONE',  ( -1.726321361862525858E-17, 3.963972222298087988, -0.2819296736111110979 ) ) ;
#7758 = AXIS2_PLACEMENT_3D ( 'NONE', #14438, #2757, #22990 ) ;
#7759 = CARTESIAN_POINT ( 'NONE',  ( 0.1202474488300702554, 4.408426576200284330, 0.2881835540050379785 ) ) ;
#7760 = CARTESIAN_POINT ( 'NONE',  ( 0.000000000000000000, 0.9099999999999988098, 0.7500000000000001110 ) ) ;
#7761 = CARTESIAN_POINT ( 'NONE',  ( 1.312321497832610059E-07, 4.821611112096344520, -0.3119999999999724105 ) ) ;
#7762 = CARTESIAN_POINT ( 'NONE',  ( 0.1954553509668047195, 0.1954553509668046085, 0.3452777777777817358 ) ) ;
#7763 = CARTESIAN_POINT ( 'NONE',  ( -0.1167790944451424506, 0.4208333332574666352, 0.2819296736111110424 ) ) ;
#7764 = CARTESIAN_POINT ( 'NONE',  ( 0.2764156081756483641, -0.1144950937579611167, -0.05402777777777704321 ) ) ;
#7765 = B_SPLINE_CURVE_WITH_KNOTS ( 'NONE', 3,
 ( #21147, #3963, #19192, #2502, #9941, #17371 ),
 .UNSPECIFIED., .F., .F.,
 ( 4, 2, 4 ),
 ( 0.000000000000000000, 0.001232805887355176112, 0.002465611774710352224 ),
 .UNSPECIFIED. ) ;
#7766 = CARTESIAN_POINT ( 'NONE',  ( 0.2819296736111110424, 5.064666666742533074, -0.1167790944451423396 ) ) ;
#7767 = CARTESIAN_POINT ( 'NONE',  ( 0.04086849681330569084, 4.461661661955456104, 0.3120000008906269051 ) ) ;
#7768 = CARTESIAN_POINT ( 'NONE',  ( -0.1993543840281266910, 4.568138888964754507, -0.1993543840281266910 ) ) ;
#7769 = CARTESIAN_POINT ( 'NONE',  ( 0.1292346314604056745, 0.2993055554038226429, -0.3119999999999999996 ) ) ;
#7770 = CARTESIAN_POINT ( 'NONE',  ( 0.2387770904324161558, 4.869557469296990959, -0.2024777428408112145 ) ) ;
#7771 = CARTESIAN_POINT ( 'NONE',  ( -0.2956994556028983423, 7.507838726391301300E-19, 0.2548636319900752789 ) ) ;
#7772 = CYLINDRICAL_SURFACE ( 'NONE', #12780, 0.3119999999999999996 ) ;
#7773 = CARTESIAN_POINT ( 'NONE',  ( -0.1292346314604057023, 4.561194444444443441, 0.3119999999999998885 ) ) ;
#7774 = CARTESIAN_POINT ( 'NONE',  ( 0.1167790944451424506, 3.759111111186976828, 0.2819296736111110424 ) ) ;
#7775 = FACE_OUTER_BOUND ( 'NONE', #790, .T. ) ;
#7776 =( BOUNDED_CURVE ( )  B_SPLINE_CURVE ( 2, ( #2661, #19716, #3019, #6918, #4604, #1310, #21787, #8735, #6431 ),
 .UNSPECIFIED., .F., .F. ) 
 B_SPLINE_CURVE_WITH_KNOTS ( ( 3, 2, 2, 2, 3 ),
 ( 0.5267857142857140795, 0.5312499999999997780, 0.5357142857142855874, 0.5401785714285712858, 0.5446428571428569843 ),
 .UNSPECIFIED. ) 
 CURVE ( )  GEOMETRIC_REPRESENTATION_ITEM ( )  RATIONAL_B_SPLINE_CURVE ( ( 1.000000000000003775, 0.9238795325112829637, 1.000000000000000000, 0.9238795325112867385, 1.000000000000000000, 0.9238795325112867385, 1.000000000000000000, 0.9238795325112886259, 0.9999999999999981126 ) ) 
 REPRESENTATION_ITEM ( '' )  );
#7777 = CARTESIAN_POINT ( 'NONE',  ( -0.3119999999999998885, 3.998694444444443885, 0.1292346314604058410 ) ) ;
#7778 = CIRCLE ( 'NONE', #373, 0.01874999999999997155 ) ;
#7779 = ORIENTED_EDGE ( 'NONE', *, *, #17225, .T. ) ;
#7780 = FACE_OUTER_BOUND ( 'NONE', #2416, .T. ) ;
#7781 = ORIENTED_EDGE ( 'NONE', *, *, #9928, .T. ) ;
#7782 = CC_DESIGN_DATE_AND_TIME_ASSIGNMENT ( #17712, #8436, ( #12722 ) ) ;
#7783 = CARTESIAN_POINT ( 'NONE',  ( -0.05621373772049894496, 4.125565998086674568, 0.3085550974868493390 ) ) ;
#7784 = CARTESIAN_POINT ( 'NONE',  ( -0.1306872919485615459, -0.3155070326520293400, -0.09048611111111044825 ) ) ;
#7785 = CARTESIAN_POINT ( 'NONE',  ( 0.2723844339573918694, 4.303051290467792889, 0.1575471963731641112 ) ) ;
#7786 = CARTESIAN_POINT ( 'NONE',  ( 0.07856389089914374291, 5.132760641740106600, 0.2966322975708292065 ) ) ;
#7787 = ORIENTED_EDGE ( 'NONE', *, *, #22172, .T. ) ;
#7788 = VECTOR ( 'NONE', #1528, 39.37007874015748854 ) ;
#7789 = CARTESIAN_POINT ( 'NONE',  ( 0.2233192592356399997, 0.07589285704531473220, -0.3073725909049500049 ) ) ;
#7790 = AXIS2_PLACEMENT_3D ( 'NONE', #6786, #6424, #17765 ) ;
#7791 = CARTESIAN_POINT ( 'NONE',  ( 0.2819296736111110424, 0.5874999999241333759, 0.1167790944451424923 ) ) ;
#7792 = CARTESIAN_POINT ( 'NONE',  ( 0.000000000000000000, 5.072999999999999510, 0.000000000000000000 ) ) ;
#7793 = CARTESIAN_POINT ( 'NONE',  ( 0.08171969123827281523, 0.7775251020733242591, -1.079850811755443951 ) ) ;
#7794 = CARTESIAN_POINT ( 'NONE',  ( 0.3108513798347909418, 0.3617957495396916245, 0.4142710792078267423 ) ) ;
#7795 = CARTESIAN_POINT ( 'NONE',  ( -0.2764156081756484196, 1.692557448933383907E-17, 0.09527777777777970969 ) ) ;
#7796 = CARTESIAN_POINT ( 'NONE',  ( 1.910449006669871087E-17, 0.4763888888888885287, -0.3119999999999999996 ) ) ;
#7797 = CARTESIAN_POINT ( 'NONE',  ( 0.3236067977499790249, 0.1124999998049151795, -0.2351141009169892826 ) ) ;
#7798 = CARTESIAN_POINT ( 'NONE',  ( -0.1292346314604056190, 0.2020833333333329485, -0.3119999999999999996 ) ) ;
#7799 = CARTESIAN_POINT ( 'NONE',  ( -0.3119999999999999996, 5.272999999999998799, 0.000000000000000000 ) ) ;
#7800 = ADVANCED_FACE ( 'NONE', ( #7775, #14870 ), #17488, .F. ) ;
#7801 = CARTESIAN_POINT ( 'NONE',  ( -0.2819296736111110979, 4.144527777853643791, 0.000000000000000000 ) ) ;
#7802 = FACE_OUTER_BOUND ( 'NONE', #12045, .T. ) ;
#7803 = CARTESIAN_POINT ( 'NONE',  ( -0.3830434977118161721, 0.3085929194348118187, 0.4166771511014252805 ) ) ;
#7804 = CARTESIAN_POINT ( 'NONE',  ( -0.001863919267159286786, 4.111524471938507119, -2.908070964936878333 ) ) ;
#7805 = ORIENTED_EDGE ( 'NONE', *, *, #16175, .T. ) ;
#7806 = VERTEX_POINT ( 'NONE', #7419 ) ;
#7807 = CARTESIAN_POINT ( 'NONE',  ( 0.3999999999999999667, 0.3160714283763437216, 0.1299678784931626307 ) ) ;
#7808 = CARTESIAN_POINT ( 'NONE',  ( 0.1167790944451422702, 4.946611111186975940, -0.2819296736111110424 ) ) ;
#7809 = EDGE_CURVE ( 'NONE', #15412, #2004, #4563, .T. ) ;
#7810 = CARTESIAN_POINT ( 'NONE',  ( -0.1116596296178199582, 0.3723214284738861068, -0.3436530038418508792 ) ) ;
#7811 = CARTESIAN_POINT ( 'NONE',  ( 0.3125000000000000000, -5.740531871003217465E-17, -0.01583333333333210996 ) ) ;
#7812 = DIRECTION ( 'NONE',  ( 0.2467484359828400198, 0.000000000000000000, 0.9690795681160667696 ) ) ;
#7813 = DIRECTION ( 'NONE',  ( 0.000000000000000000, 0.000000000000000000, 1.000000000000000000 ) ) ;
#7814 = CARTESIAN_POINT ( 'NONE',  ( 0.000000000000000000, 6.000000000000000888, 0.000000000000000000 ) ) ;
#7815 = CARTESIAN_POINT ( 'NONE',  ( 0.2819296736111111534, 4.224388888964755395, 0.1167790944451422563 ) ) ;
#7816 = CALENDAR_DATE ( 2026, 7, 10 ) ;
#7817 = CARTESIAN_POINT ( 'NONE',  ( 0.8977114317029943891, 2.291712385858714729, -0.6297771125693037986 ) ) ;
#7818 = CARTESIAN_POINT ( 'NONE',  ( -0.1954553509668046918, -0.1954553509668046640, -0.06444444444444380471 ) ) ;
#7819 = CARTESIAN_POINT ( 'NONE',  ( 0.1236067977499789861, 0.2714285714285713524, -0.3804226065180614236 ) ) ;
#7820 = CARTESIAN_POINT ( 'NONE',  ( 0.1993543840281266910, 0.3895833332574666352, -0.1993543840281266910 ) ) ;
#7821 = LINE ( 'NONE', #381, #14050 ) ;
#7822 = CARTESIAN_POINT ( 'NONE',  ( 0.3236067977499789694, 0.1785714285714284921, 0.2351141009169893659 ) ) ;
#7823 = CARTESIAN_POINT ( 'NONE',  ( -3.863846776457871776E-17, -0.3155070326520292845, 0.2428472222222251287 ) ) ;
#7824 = CARTESIAN_POINT ( 'NONE',  ( 0.4687500000000003886, 0.08771909047139087034, 0.4143497438722636428 ) ) ;
#7825 = CARTESIAN_POINT ( 'NONE',  ( 0.1292346314603988466, 5.033416666666665762, -0.3120000000000067164 ) ) ;
#7826 = CARTESIAN_POINT ( 'NONE',  ( -0.2819296736111110979, 0.3930555554796889561, -0.1167790944451423396 ) ) ;
#7827 = CARTESIAN_POINT ( 'NONE',  ( -0.1993543840281267465, 0.1812499999241333759, 0.1993543840281266633 ) ) ;
#7828 = ADVANCED_FACE ( 'NONE', ( #2736 ), #16687, .F. ) ;
#7829 = CARTESIAN_POINT ( 'NONE',  ( -0.1167790944451423257, 4.356333333409199149, -0.2819296736111110424 ) ) ;
#7830 = CARTESIAN_POINT ( 'NONE',  ( -0.3236067977499789694, 0.4196428569477723136, -0.2351141009169893104 ) ) ;
#7831 = CARTESIAN_POINT ( 'NONE',  ( -0.1993543840281266355, 4.929250000075866112, 0.1993543840281267465 ) ) ;
#7832 = CARTESIAN_POINT ( 'NONE',  ( -1.726321361862525858E-17, 4.227861111186976828, -0.2819296736111110979 ) ) ;
#7833 = CARTESIAN_POINT ( 'NONE',  ( 0.3125000000000002220, -0.1294417382415921358, 0.3140277777777816803 ) ) ;
#7834 = CARTESIAN_POINT ( 'NONE',  ( -0.1294417382415922746, -0.3125000000000000000, 0.2376388888888918416 ) ) ;
#7835 = CARTESIAN_POINT ( 'NONE',  ( -0.1292346314604056745, 3.991750000151732980, -0.3119999999999999996 ) ) ;
#7836 = EDGE_CURVE ( 'NONE', #10167, #19328, #11201, .T. ) ;
#7837 = LINE ( 'NONE', #20763, #6400 ) ;
#7838 = ORIENTED_EDGE ( 'NONE', *, *, #18127, .T. ) ;
#7839 = CALENDAR_DATE ( 2026, 7, 10 ) ;
#7840 = CARTESIAN_POINT ( 'NONE',  ( 0.06796888784162435915, 0.2795977689546983447, 0.3992516814463595298 ) ) ;
#7841 = LINE ( 'NONE', #15288, #17342 ) ;
#7842 = CARTESIAN_POINT ( 'NONE',  ( -0.2256660336270156497, 5.008917305905795203, 0.2154793158332795333 ) ) ;
#7843 = ORIENTED_EDGE ( 'NONE', *, *, #14237, .T. ) ;
#7844 = CARTESIAN_POINT ( 'NONE',  ( 0.3119999999999998885, 0.5076388887371560132, 0.1292346314604058410 ) ) ;
#7845 = ORIENTED_EDGE ( 'NONE', *, *, #14566, .T. ) ;
#7846 = DIRECTION ( 'NONE',  ( -0.000000000000000000, -1.000000000000000000, -0.000000000000000000 ) ) ;
#7847 = CARTESIAN_POINT ( 'NONE',  ( 1.964169762594504265, 2.687712728237018567, -2.661240473580835708 ) ) ;
#7848 = CARTESIAN_POINT ( 'NONE',  ( -0.1292346314604056190, 0.5354166666666663188, -0.3119999999999999996 ) ) ;
#7849 = CARTESIAN_POINT ( 'NONE',  ( 0.2923287055106771337, 0.1294642856167433076, 0.2123892367102621359 ) ) ;
#7850 = CARTESIAN_POINT ( 'NONE',  ( 0.2335907231169286336, 5.183691625336232178, -0.1757699240049868106 ) ) ;
#7851 = ORIENTED_EDGE ( 'NONE', *, *, #16115, .T. ) ;
#7852 = CARTESIAN_POINT ( 'NONE',  ( 2.326421213736078119E-17, 0.3866071427596002863, -0.3799334167787516980 ) ) ;
#7853 = EDGE_LOOP ( 'NONE', ( #5772, #5777, #3225, #18970 ) ) ;
#7854 = CARTESIAN_POINT ( 'NONE',  ( 3.887228417612631703E-07, 4.154944433789834690, -0.3119999999997578044 ) ) ;
#7855 = CARTESIAN_POINT ( 'NONE',  ( -0.2307680606616751562, 4.675378956632738614, 0.2099770340440785255 ) ) ;
#7856 = CARTESIAN_POINT ( 'NONE',  ( 0.2819296736111110979, 3.991750000075865223, -3.452642723725051716E-17 ) ) ;
#7857 = CARTESIAN_POINT ( 'NONE',  ( 3.194613732291736063, 1.301349684034776022, -3.842349684034790602 ) ) ;
#7858 = CARTESIAN_POINT ( 'NONE',  ( -0.3147071693084031452, 0.3721877333702313662, 0.07155713030921627416 ) ) ;
#7859 = CARTESIAN_POINT ( 'NONE',  ( 0.4749999999999999778, 3.575000000000000622, -0.09499999999999995948 ) ) ;
#7860 = CARTESIAN_POINT ( 'NONE',  ( 0.2206173157302027954, 4.648000000151731648, -0.2206173157302028232 ) ) ;
#7861 = CARTESIAN_POINT ( 'NONE',  ( -0.1167790944451423119, 4.856333333409199149, -0.2819296736111110979 ) ) ;
#7862 = ORIENTED_EDGE ( 'NONE', *, *, #11812, .F. ) ;
#7863 = CARTESIAN_POINT ( 'NONE',  ( -0.2819296736111110979, 4.241750000075865223, 0.000000000000000000 ) ) ;
#7864 = ORIENTED_EDGE ( 'NONE', *, *, #12330, .T. ) ;
#7865 = CARTESIAN_POINT ( 'NONE',  ( 2.326421213736078119E-17, 0.08303571418817184968, -0.3799334167787516980 ) ) ;
#7866 = ORIENTED_EDGE ( 'NONE', *, *, #11555, .F. ) ;
#7867 = VERTEX_POINT ( 'NONE', #16810 ) ;
#7868 = CALENDAR_DATE ( 2026, 7, 10 ) ;
#7869 = CARTESIAN_POINT ( 'NONE',  ( 0.3155070326520292290, -0.1306872919485616569, 0.4234027777777825130 ) ) ;
#7870 = DIRECTION ( 'NONE',  ( 0.000000000000000000, 0.000000000000000000, -1.000000000000000000 ) ) ;
#7871 = CARTESIAN_POINT ( 'NONE',  ( 0.2819296736111110979, 3.953555555631421470, -0.1167790944451423396 ) ) ;
#7872 = CARTESIAN_POINT ( 'NONE',  ( 0.09525661631228125870, 4.429985109478741023, -0.2971466434106878607 ) ) ;
#7873 = CARTESIAN_POINT ( 'NONE',  ( 0.3119999999999999996, 4.637583333333332725, -0.1292346314604056745 ) ) ;
#7874 = CARTESIAN_POINT ( 'NONE',  ( 0.1965595339003342046, -0.4277821775561181927, 0.07944544255959536116 ) ) ;
#7875 = CARTESIAN_POINT ( 'NONE',  ( -0.1144950937579609779, 0.2764156081756484196, 0.1890277777777804868 ) ) ;
#7876 = CARTESIAN_POINT ( 'NONE',  ( 0.1167790944451423119, 0.5597222221463556968, -0.2819296736111110979 ) ) ;
#7877 = CARTESIAN_POINT ( 'NONE',  ( 0.1144950937579609085, -0.2764156081756484751, 0.4459722222222269328 ) ) ;
#7878 = ORIENTED_EDGE ( 'NONE', *, *, #16716, .T. ) ;
#7879 = CARTESIAN_POINT ( 'NONE',  ( 0.2819296736111110979, 4.672305555631421470, -3.452642723725051716E-17 ) ) ;
#7880 = AXIS2_PLACEMENT_3D ( 'NONE', #19847, #10595, #18023 ) ;
#7881 = CARTESIAN_POINT ( 'NONE',  ( 0.2819296736111110979, 4.658416666742532186, -3.452642723725051716E-17 ) ) ;
#7882 = CARTESIAN_POINT ( 'NONE',  ( -0.1376066337087289981, 0.2509841804965734502, -0.07524251643492650687 ) ) ;
#7883 = LINE ( 'NONE', #15335, #8575 ) ;
#7884 = FACE_OUTER_BOUND ( 'NONE', #8547, .T. ) ;
#7885 = CARTESIAN_POINT ( 'NONE',  ( 1.766928915791902144, 2.471730513698206178, -1.986411895277231832 ) ) ;
#7886 = CARTESIAN_POINT ( 'NONE',  ( -0.3119999999999998885, 4.443138888888888083, 0.1292346314604058410 ) ) ;
#7887 = CARTESIAN_POINT ( 'NONE',  ( 1.750236327630675475E-17, 0.2749999999999999112, -0.3999999999999999667 ) ) ;
#7888 = EDGE_CURVE ( 'NONE', #19306, #8464, #91, .T. ) ;
#7889 = CARTESIAN_POINT ( 'NONE',  ( -0.2206173157302028232, 3.988277777777776922, -0.2206173157302028232 ) ) ;
#7890 = ORIENTED_EDGE ( 'NONE', *, *, #23902, .F. ) ;
#7891 = DIRECTION ( 'NONE',  ( 1.000000000000000000, 0.000000000000000000, 0.000000000000000000 ) ) ;
#7892 = ORIENTED_EDGE ( 'NONE', *, *, #11697, .T. ) ;
#7893 = CARTESIAN_POINT ( 'NONE',  ( 0.2828379296212147898, 4.700474317598876794, -0.1317075689354028911 ) ) ;
#7894 = VECTOR ( 'NONE', #22013, 39.37007874015747433 ) ;
#7895 = CARTESIAN_POINT ( 'NONE',  ( 0.001541891433799943327, 4.654900223093500600, -0.3119964281628413993 ) ) ;
#7896 = CARTESIAN_POINT ( 'NONE',  ( 0.2764156081756483641, 0.1144950937579610056, 0.4529166666666715191 ) ) ;
#7897 = CARTESIAN_POINT ( 'NONE',  ( 0.1918605058169607913, 4.315775238200347808, -0.2494071876536460841 ) ) ;
#7898 = ORIENTED_EDGE ( 'NONE', *, *, #17465, .F. ) ;
#7899 = CARTESIAN_POINT ( 'NONE',  ( 0.2923287055106771337, -0.01339285724039953988, 0.2123892367102621359 ) ) ;
#7900 = CARTESIAN_POINT ( 'NONE',  ( -5.178964085587577574E-17, 0.5215277777019111660, 0.2819296736111110979 ) ) ;
#7901 = DIRECTION ( 'NONE',  ( -0.000000000000000000, -1.000000000000000000, -0.000000000000000000 ) ) ;
#7902 = CARTESIAN_POINT ( 'NONE',  ( 0.04131066265099773288, 0.1822999795785922583, -1.241739854591859871 ) ) ;
#7903 = CARTESIAN_POINT ( 'NONE',  ( -5.731347020009612645E-17, 0.1708333333333330040, 0.3119999999999999996 ) ) ;
#7904 = CARTESIAN_POINT ( 'NONE',  ( 0.1954553509668046640, -0.1954553509668047195, 0.2272222222222252119 ) ) ;
#7905 =( BOUNDED_CURVE ( )  B_SPLINE_CURVE ( 2, ( #2488, #282, #17355, #21007, #15646, #8196, #9806 ),
 .UNSPECIFIED., .F., .T. ) 
 B_SPLINE_CURVE_WITH_KNOTS ( ( 3, 2, 2, 3 ),
 ( 0.9642857142857143016, 0.9714285714285714191, 0.9857142857142857650, 1.000000000000000000 ),
 .UNSPECIFIED. ) 
 CURVE ( )  GEOMETRIC_REPRESENTATION_ITEM ( )  RATIONAL_B_SPLINE_CURVE ( ( 0.9755282581475768211, 0.9755282581475768211, 1.000000000000000000, 0.9510565162951535312, 1.000000000000000000, 0.9510565162951535312, 1.000000000000000000 ) ) 
 REPRESENTATION_ITEM ( '' )  );
#7906 = CARTESIAN_POINT ( 'NONE',  ( -0.3106743519353148963, 4.612164334677839150, -0.03847270028753647930 ) ) ;
#7907 = CARTESIAN_POINT ( 'NONE',  ( 0.000000000000000000, 3.700000000000000622, 0.000000000000000000 ) ) ;
#7908 = CARTESIAN_POINT ( 'NONE',  ( 0.1294417382415924134, 0.3124999999999999445, 0.3279166666666706864 ) ) ;
#7909 = CARTESIAN_POINT ( 'NONE',  ( -0.3119999999999999996, 0.3236111111111107941, -3.820898013339742174E-17 ) ) ;
#7910 = CARTESIAN_POINT ( 'NONE',  ( 0.3119999999999999996, 5.189666666666666650, -3.820898013339742174E-17 ) ) ;
#7911 = VECTOR ( 'NONE', #19039, 39.37007874015748143 ) ;
#7912 = CARTESIAN_POINT ( 'NONE',  ( -0.2819296736111110424, 4.307722222298088433, -0.1167790944451423119 ) ) ;
#7913 = CARTESIAN_POINT ( 'NONE',  ( 0.2730879860166530726, 3.066692553488282957, 2.936183489075822717 ) ) ;
#7914 = CARTESIAN_POINT ( 'NONE',  ( 0.4172595264191667486, 2.291712385858714285, -0.8269699969948853813 ) ) ;
#7915 = CARTESIAN_POINT ( 'NONE',  ( 1.038941561183303497, 3.066692553488282957, 0.8003320438460471697 ) ) ;
#7916 = EDGE_LOOP ( 'NONE', ( #22829, #1160, #10521, #14711, #15082, #18235, #9202, #14626, #12826, #13265 ) ) ;
#7917 = ORIENTED_EDGE ( 'NONE', *, *, #1423, .F. ) ;
#7918 = FACE_OUTER_BOUND ( 'NONE', #4535, .T. ) ;
#7919 = CARTESIAN_POINT ( 'NONE',  ( -0.1167790944451423535, 4.752166666742533074, 0.2819296736111110424 ) ) ;
#7920 = CARTESIAN_POINT ( 'NONE',  ( -0.1334452016168097832, 5.163863756405055128, 0.2677057760511410422 ) ) ;
#7921 = B_SPLINE_CURVE_WITH_KNOTS ( 'NONE', 3,
 ( #20409, #1994, #9431, #11148, #16751, #759, #21002, #1123, #13590, #17833, #17467, #641 ),
 .UNSPECIFIED., .F., .F.,
 ( 4, 2, 2, 2, 2, 4 ),
 ( 0.000000000000000000, 0.003345931539952393900, 0.005018897309928590199, 0.006691863079904788666, 0.01003779461985718560, 0.01338372615980958080 ),
 .UNSPECIFIED. ) ;
#7922 = CARTESIAN_POINT ( 'NONE',  ( 7.192576327740195730, 4.466718170109853503, -2.843237311110146770 ) ) ;
#7923 = FACE_OUTER_BOUND ( 'NONE', #21157, .T. ) ;
#7924 = CARTESIAN_POINT ( 'NONE',  ( 0.1167790944451424506, 4.328555555631421470, 0.2819296736111110424 ) ) ;
#7925 = PERSON_AND_ORGANIZATION_ROLE ( 'classification_officer' ) ;
#7926 = AXIS2_PLACEMENT_3D ( 'NONE', #9904, #747, #6355 ) ;
#7927 = CARTESIAN_POINT ( 'NONE',  ( 0.2206173157302028787, 4.293833333333332725, 0.2206173157302027954 ) ) ;
#7928 = CARTESIAN_POINT ( 'NONE',  ( -3.385114897866767815E-17, -0.2764156081756484196, 0.05361111111111271227 ) ) ;
#7929 = LINE ( 'NONE', #11856, #7911 ) ;
#7930 = EDGE_LOOP ( 'NONE', ( #15727, #6718 ) ) ;
#7931 = CARTESIAN_POINT ( 'NONE',  ( 0.2819296736111110424, 0.4972222221463556413, -0.1167790944451423119 ) ) ;
#7932 = CARTESIAN_POINT ( 'NONE',  ( 5.731347020009612645E-17, 4.120222222222221120, 0.3119999999999999996 ) ) ;
#7933 = CARTESIAN_POINT ( 'NONE',  ( 3.820898013339742174E-17, 5.384999999999999787, 0.3119999999999999996 ) ) ;
#7934 = CARTESIAN_POINT ( 'NONE',  ( -0.1236067977499789583, 0.1357142857142856485, -0.3804226065180614791 ) ) ;
#7935 = CARTESIAN_POINT ( 'NONE',  ( -0.2230971623002954152, -0.2230971623002953874, 0.1247916666666686186 ) ) ;
#7936 = EDGE_CURVE ( 'NONE', #18537, #1154, #17730, .T. ) ;
#7937 = CARTESIAN_POINT ( 'NONE',  ( -0.2195630361087207438, -0.1679215936615484350, -0.06558227484231504700 ) ) ;
#7938 = CARTESIAN_POINT ( 'NONE',  ( 0.2819296736111110979, 0.5354166665908000056, 0.000000000000000000 ) ) ;
#7939 = CARTESIAN_POINT ( 'NONE',  ( 0.1167790944451423535, 0.2472222221463555303, 0.2819296736111110424 ) ) ;
#7940 = CARTESIAN_POINT ( 'NONE',  ( 0.1993543840281266633, 4.345916666742532186, -0.1993543840281266910 ) ) ;
#7941 = CARTESIAN_POINT ( 'NONE',  ( 2.575339694675500462E-17, 0.3374999998049151850, -0.4205848896953069405 ) ) ;
#7942 = CARTESIAN_POINT ( 'NONE',  ( 0.1993543840281266633, 4.957027777853642903, -0.1993543840281266910 ) ) ;
#7943 = CARTESIAN_POINT ( 'NONE',  ( 0.1993543840281267465, 4.151472222298087544, 0.1993543840281266633 ) ) ;
#7944 = CARTESIAN_POINT ( 'NONE',  ( 2.336126731229780429, 2.690142902515283208, -2.565857097484717020 ) ) ;
#7945 = PERSON ( 'NAUO-PER9', 'UNSPECIFIED', 'UNSPECIFIED', ('UNSPECIFIED'), ('UNSPECIFIED'), ('UNSPECIFIED') ) ;
#7946 = VERTEX_POINT ( 'NONE', #14319 ) ;
#7947 = CARTESIAN_POINT ( 'NONE',  ( 0.000000000000000000, 0.3125000000000000000, 0.1022222222222240184 ) ) ;
#7948 = CARTESIAN_POINT ( 'NONE',  ( -0.1292346314604056745, 3.825083333485065129, -0.3119999999999999996 ) ) ;
#7949 = AXIS2_PLACEMENT_3D ( 'NONE', #15877, #23293, #4770 ) ;
#7950 = CARTESIAN_POINT ( 'NONE',  ( -0.3999999999999999667, 0.2803571426620579676, -0.1299678784931626030 ) ) ;
#7951 = APPLICATION_CONTEXT ( 'configuration controlled 3d designs of mechanical parts and assemblies' ) ;
#7952 = SHAPE_REPRESENTATION ( 'Aloris-BXA-Center-Rod', ( #9127 ), #15765 ) ;
#7953 = CARTESIAN_POINT ( 'NONE',  ( -0.2236587330423011055, -0.2167494423014863503, -0.1001684177326861991 ) ) ;
#7954 = EDGE_LOOP ( 'NONE', ( #13374, #8460, #18853, #11689 ) ) ;
#7955 =( GEOMETRIC_REPRESENTATION_CONTEXT ( 3 ) GLOBAL_UNCERTAINTY_ASSIGNED_CONTEXT ( ( #23356 ) ) GLOBAL_UNIT_ASSIGNED_CONTEXT ( ( #17469, #19295, #1002 ) ) REPRESENTATION_CONTEXT ( 'NONE', 'WORKASPACE' ) );
#7956 = EDGE_CURVE ( 'NONE', #18530, #19679, #4773, .T. ) ;
#7957 = MECHANICAL_CONTEXT ( 'NONE', #8407, 'mechanical' ) ;
#7958 = CARTESIAN_POINT ( 'NONE',  ( 0.2800968539712072602, -5.145295735006237905E-17, 0.3917635206378741186 ) ) ;
#7959 = CARTESIAN_POINT ( 'NONE',  ( -0.1552057294347528038, 5.011424740845276560, 0.2737342765630598751 ) ) ;
#7960 = VERTEX_POINT ( 'NONE', #10306 ) ;
#7961 = CARTESIAN_POINT ( 'NONE',  ( -0.2819296736111110424, 0.01805555547968892491, -0.1167790944451423396 ) ) ;
#7962 = ORIENTED_EDGE ( 'NONE', *, *, #19287, .F. ) ;
#7963 = CARTESIAN_POINT ( 'NONE',  ( -0.3999999999999999667, 0.003571428571428547898, -0.1299678784931626030 ) ) ;
#7964 = CARTESIAN_POINT ( 'NONE',  ( 0.009374999999999843528, 0.5358532185916217161, 0.3779506566538944345 ) ) ;
#7965 = CARTESIAN_POINT ( 'NONE',  ( 0.1154082656451064642, 4.762710407878993912, -0.2907850784680934830 ) ) ;
#7966 = AXIS2_PLACEMENT_3D ( 'NONE', #23145, #6457, #21455 ) ;
#7967 = CARTESIAN_POINT ( 'NONE',  ( -6.979263641208234666E-17, 0.04732142847388615819, 0.3799334167787516425 ) ) ;
#7968 = CARTESIAN_POINT ( 'NONE',  ( 0.2214705455607580142, 5.184159519586463816, -0.1905467935019724002 ) ) ;
#7969 = EDGE_CURVE ( 'NONE', #14969, #13125, #7778, .T. ) ;
#7970 = ORIENTED_EDGE ( 'NONE', *, *, #21096, .F. ) ;
#7971 = CARTESIAN_POINT ( 'NONE',  ( -0.3613381517857143232, 0.3294642856167431799, -0.1174058825155741143 ) ) ;
#7972 = DIRECTION ( 'NONE',  ( -0.000000000000000000, -1.000000000000000000, -0.000000000000000000 ) ) ;
#7973 = CARTESIAN_POINT ( 'NONE',  ( -0.1292346314604081170, 4.040361111111110404, -0.3119999999999975016 ) ) ;
#7974 = CARTESIAN_POINT ( 'NONE',  ( -0.1993543840281266355, 4.026472222298087544, 0.1993543840281267465 ) ) ;
#7975 = DIRECTION ( 'NONE',  ( -0.3273051541876813575, -0.6681584153635157231, 0.6681584153635227175 ) ) ;
#7976 = APPROVAL_PERSON_ORGANIZATION ( #9436, #6729, #160 ) ;
#7977 = CARTESIAN_POINT ( 'NONE',  ( -0.1298740736329927759, 5.192253054662280043, 0.2575819732643157001 ) ) ;
#7978 = CARTESIAN_POINT ( 'NONE',  ( -0.1292346314604056745, 4.713972222373954857, -0.3119999999999999996 ) ) ;
#7979 = CARTESIAN_POINT ( 'NONE',  ( 0.1167790944451424506, 4.995222222298087544, 0.2819296736111110424 ) ) ;
#7980 = CARTESIAN_POINT ( 'NONE',  ( 0.1993543840281267465, 4.262583333409199149, 0.1993543840281266633 ) ) ;
#7981 = EDGE_LOOP ( 'NONE', ( #2283, #8338 ) ) ;
#7982 = CARTESIAN_POINT ( 'NONE',  ( 0.3613381517857143232, 0.1366071427596004251, 0.000000000000000000 ) ) ;
#7983 = VECTOR ( 'NONE', #3743, 39.37007874015748143 ) ;
#7984 = ORIENTED_EDGE ( 'NONE', *, *, #9464, .T. ) ;
#7985 = EDGE_CURVE ( 'NONE', #10268, #21333, #18091, .T. ) ;
#7986 = EDGE_LOOP ( 'NONE', ( #4897, #16926, #3995, #20064 ) ) ;
#7987 = DATE_AND_TIME ( #17382, #18900 ) ;
#7988 = CARTESIAN_POINT ( 'NONE',  ( 0.4620259694561523744, 0.2880908832651559726, 0.04413116910601654758 ) ) ;
#7989 = CARTESIAN_POINT ( 'NONE',  ( -0.7171867353193368544, 0.9548081934128058723, 2.866728992292166378 ) ) ;
#7990 = LOCAL_TIME ( 21, 9, 13.00000000000000000, #18583 ) ;
#7991 = CARTESIAN_POINT ( 'NONE',  ( 1.910449006669871087E-17, 0.1361111109593781676, -0.3119999999999999996 ) ) ;
#7992 = CARTESIAN_POINT ( 'NONE',  ( 0.1423755856867760516, 4.428580575607206526, -0.2791577753537264894 ) ) ;
#7993 = CARTESIAN_POINT ( 'NONE',  ( -1.910449006669871087E-17, 4.425777777777777366, -0.3119999999999999996 ) ) ;
#7994 = B_SPLINE_CURVE_WITH_KNOTS ( 'NONE', 3,
 ( #7958, #20889, #17238, #4421, #2245, #10049, #765, #22603, #5887, #13822, #21256, #4543, #19420, #9679, #13348, #20770, #4059, #17118, #405, #7840, #17688, #6954, #18168, #16343, #981, #14515, #4991, #12455, #15977, #23514, #23398, #21936, #16100, #3052, #2930, #6587, #14150, #4750, #19514, #21579, #6706, #23637, #4874, #17929 ),
 .UNSPECIFIED., .F., .F.,
 ( 4, 2, 1, 2, 2, 2, 2, 2, 2, 1, 2, 2, 2, 2, 2, 2, 2, 2, 2, 2, 2, 2, 4 ),
 ( 0.004595939250188698158, 0.005313238532189881215, 0.006030537814191064272, 0.006747837096192247329, 0.007465136378193430386, 0.008899734942195796500, 0.01033433350619816435, 0.01176893207020052873, 0.01248623135220171265, 0.01320353063420289484, 0.01392082991620407877, 0.01463812919820526096, 0.01607272776220762533, 0.01750732632620999318, 0.01894192489021236103, 0.01965922417221354149, 0.02037652345421472194, 0.02181112201821708979, 0.02324572058221945764, 0.02396301986422064156, 0.02468031914622182549, 0.02611491771022419334, 0.02754951627422656119 ),
 .UNSPECIFIED. ) ;
#7995 = CARTESIAN_POINT ( 'NONE',  ( 0.03284172987836220248, 0.06131004178175258196, 0.3095030519831387661 ) ) ;
#7996 = CARTESIAN_POINT ( 'NONE',  ( -0.2764156081756484196, 0.1144950937579609918, 0.1959722222222249899 ) ) ;
#7997 = CARTESIAN_POINT ( 'NONE',  ( -5.178964085587577574E-17, 0.5354166665908000056, 0.2819296736111110979 ) ) ;
#7998 = CARTESIAN_POINT ( 'NONE',  ( 0.2764156081756483641, 0.1144950937579610056, 0.4598611111111158833 ) ) ;
#7999 = ORIENTED_EDGE ( 'NONE', *, *, #20136, .T. ) ;
#8000 = CARTESIAN_POINT ( 'NONE',  ( 0.1167790944451422702, 4.738277777853642903, -0.2819296736111110424 ) ) ;
#8001 = CARTESIAN_POINT ( 'NONE',  ( 0.004206913933137047291, -0.5383631510497720596, 0.04698599556840569319 ) ) ;
#8002 = CARTESIAN_POINT ( 'NONE',  ( -0.2819296736111110979, 4.741750000075865223, 0.000000000000000000 ) ) ;
#8003 = CARTESIAN_POINT ( 'NONE',  ( -0.05067229266822954187, 4.156391035130668321, -0.3080256783650057728 ) ) ;
#8004 = CARTESIAN_POINT ( 'NONE',  ( 0.2912189908955998274, 4.866517260218439667, -0.1119643521765174149 ) ) ;
#8005 = LINE ( 'NONE', #4346, #10224 ) ;
#8006 = CARTESIAN_POINT ( 'NONE',  ( 1.791833110003796271E-17, 0.04312855400452411669, -0.2926285540045244216 ) ) ;
#8007 = CARTESIAN_POINT ( 'NONE',  ( -0.1292346314604057023, 4.227861111111110404, 0.3119999999999998885 ) ) ;
#8008 = CARTESIAN_POINT ( 'NONE',  ( -0.2819296736111110979, 3.852861111186976828, 0.000000000000000000 ) ) ;
#8009 = PRODUCT_DEFINITION_FORMATION_WITH_SPECIFIED_SOURCE ( 'ANY', '', #3495, .NOT_KNOWN. ) ;
#8010 = ORIENTED_EDGE ( 'NONE', *, *, #2129, .T. ) ;
#8011 = CARTESIAN_POINT ( 'NONE',  ( 0.3133650935564305517, 4.586437319524496736, -0.03335398037977004015 ) ) ;
#8012 = VERTEX_POINT ( 'NONE', #23680 ) ;
#8013 = CARTESIAN_POINT ( 'NONE',  ( 0.3125000000000000000, -5.740531871003217465E-17, 0.09527777777777987622 ) ) ;
#8014 = AXIS2_PLACEMENT_3D ( 'NONE', #13202, #20615, #3915 ) ;
#8015 = CARTESIAN_POINT ( 'NONE',  ( 0.2260310869702762682, 4.147801854619606488, -0.2186894788897151554 ) ) ;
#8016 = CARTESIAN_POINT ( 'NONE',  ( -0.3155070326520293400, 0.1306872919485614903, -0.1043749999999994543 ) ) ;
#8017 = EDGE_CURVE ( 'NONE', #7263, #19306, #21869, .T. ) ;
#8018 = FACE_OUTER_BOUND ( 'NONE', #14095, .T. ) ;
#8019 = ADVANCED_FACE ( 'NONE', ( #23320 ), #16024, .F. ) ;
#8020 = ORIENTED_EDGE ( 'NONE', *, *, #17324, .F. ) ;
#8021 = CARTESIAN_POINT ( 'NONE',  ( 0.2233192592356399997, -0.06696428581182808926, -0.3073725909049500049 ) ) ;
#8022 = CARTESIAN_POINT ( 'NONE',  ( 0.1167790944451423535, 0.4138888888130222155, 0.2819296736111110424 ) ) ;
#8023 = CARTESIAN_POINT ( 'NONE',  ( 3.073863465859856523E-17, 5.579732050807569621, 0.2510000000000000009 ) ) ;
#8024 = CARTESIAN_POINT ( 'NONE',  ( 0.3236067977499790249, 0.04107142837634377569, -0.2351141009169892826 ) ) ;
#8025 = CARTESIAN_POINT ( 'NONE',  ( -0.1054825322677925281, -0.2618223909956075013, -0.07090283079844149350 ) ) ;
#8026 = CARTESIAN_POINT ( 'NONE',  ( -0.2764156081756484196, 0.1144950937579609918, 0.2584722222222254340 ) ) ;
#8027 = EDGE_LOOP ( 'NONE', ( #20533, #1648, #3415 ) ) ;
#8028 = CARTESIAN_POINT ( 'NONE',  ( -0.2339481197358992404, 5.111336026920037412, 0.2038494990519414962 ) ) ;
#8029 = CARTESIAN_POINT ( 'NONE',  ( 0.1236067977499789861, 0.1196428569477723386, -0.3804226065180614236 ) ) ;
#8030 = CARTESIAN_POINT ( 'NONE',  ( 0.2934658712818546955, -2.697513918649167310E-18, -0.2160150187107265918 ) ) ;
#8031 = CARTESIAN_POINT ( 'NONE',  ( 0.3119999999999998885, 0.1812499999999996614, 0.1292346314604058410 ) ) ;
#8032 = CARTESIAN_POINT ( 'NONE',  ( 0.3119999999999999996, 4.911888888888888083, -3.820898013339742174E-17 ) ) ;
#8033 = VECTOR ( 'NONE', #10972, 39.37007874015748143 ) ;
#8034 = CARTESIAN_POINT ( 'NONE',  ( 0.1167790944451424368, 4.217444444520310753, 0.2819296736111110424 ) ) ;
#8035 = LINE ( 'NONE', #11836, #12791 ) ;
#8036 = DIRECTION ( 'NONE',  ( 0.000000000000000000, -0.000000000000000000, 1.000000000000000000 ) ) ;
#8037 = DIRECTION ( 'NONE',  ( 0.000000000000000000, 1.000000000000000000, 0.000000000000000000 ) ) ;
#8038 = ORIENTED_EDGE ( 'NONE', *, *, #14595, .F. ) ;
#8039 = ORIENTED_EDGE ( 'NONE', *, *, #18738, .F. ) ;
#8040 = DIRECTION ( 'NONE',  ( -0.000000000000000000, -1.000000000000000000, -0.000000000000000000 ) ) ;
#8041 = CARTESIAN_POINT ( 'NONE',  ( -0.1993543840281266355, 4.804250000075865223, 0.1993543840281267465 ) ) ;
#8042 = CARTESIAN_POINT ( 'NONE',  ( 0.1116596296178199860, 0.3651785713310289894, -0.3436530038418508792 ) ) ;
#8043 = CARTESIAN_POINT ( 'NONE',  ( 0.4225900379021583775, -0.2972834052256092541, 0.3902123106865083013 ) ) ;
#8044 = CARTESIAN_POINT ( 'NONE',  ( -0.4687500000000003886, -0.2150850509746254080, 0.05816300916149743511 ) ) ;
#8045 = APPROVAL ( #7514, 'UNSPECIFIED' ) ;
#8046 = CARTESIAN_POINT ( 'NONE',  ( 0.1292346314604056745, 0.6326388887371557912, -0.3119999999999999996 ) ) ;
#8047 = AXIS2_PLACEMENT_3D ( 'NONE', #21108, #13448, #9655 ) ;
#8048 = CARTESIAN_POINT ( 'NONE',  ( 0.1167790944451424506, 4.384111111186976828, 0.2819296736111110424 ) ) ;
#8049 = DIRECTION ( 'NONE',  ( 1.000000000000000000, 0.000000000000000000, 0.000000000000000000 ) ) ;
#8050 =( BOUNDED_CURVE ( )  B_SPLINE_CURVE ( 1, ( #9499, #12641 ),
 .UNSPECIFIED., .F., .F. ) 
 B_SPLINE_CURVE_WITH_KNOTS ( ( 2, 2 ),
 ( 0.000000000000000000, 1.000000000000000000 ),
 .UNSPECIFIED. ) 
 CURVE ( )  GEOMETRIC_REPRESENTATION_ITEM ( )  RATIONAL_B_SPLINE_CURVE ( ( 0.9836825870399050764, 0.9836825870399050764 ) ) 
 REPRESENTATION_ITEM ( '' )  );
#8051 = CARTESIAN_POINT ( 'NONE',  ( 0.1144950937579609085, -0.2764156081756484751, -0.05402777777777704321 ) ) ;
#8052 =( BOUNDED_CURVE ( )  B_SPLINE_CURVE ( 2, ( #9462, #9342, #3733, #5679, #16895, #16784, #65, #3853, #9583 ),
 .UNSPECIFIED., .F., .T. ) 
 B_SPLINE_CURVE_WITH_KNOTS ( ( 3, 2, 2, 2, 3 ),
 ( 0.6458333333333333703, 0.6562500000000000000, 0.6666666666666666297, 0.6770833333333333703, 0.6875000000000000000 ),
 .UNSPECIFIED. ) 
 CURVE ( )  GEOMETRIC_REPRESENTATION_ITEM ( )  RATIONAL_B_SPLINE_CURVE ( ( 1.000000000000000000, 0.9238795325112867385, 1.000000000000000000, 0.9238795325112867385, 1.000000000000000000, 0.9238795325112867385, 1.000000000000000000, 0.9238795325112867385, 1.000000000000000000 ) ) 
 REPRESENTATION_ITEM ( '' )  );
#8053 = CARTESIAN_POINT ( 'NONE',  ( -0.3125000000000002776, -0.1294417382415919415, 0.3487500000000041678 ) ) ;
#8054 = VERTEX_POINT ( 'NONE', #17857 ) ;
#8055 = CARTESIAN_POINT ( 'NONE',  ( -0.1167790944451422702, 0.4555555554796890116, -0.2819296736111110424 ) ) ;
#8056 = CARTESIAN_POINT ( 'NONE',  ( 0.4700000000000001954, 2.740000000000000213, -1.836096189432333103 ) ) ;
#8057 = CARTESIAN_POINT ( 'NONE',  ( -0.3999999999999999667, 0.1464285714285713802, -0.1299678784931626030 ) ) ;
#8058 = CARTESIAN_POINT ( 'NONE',  ( -0.2472135954999579444, 0.3535714285714284810, -0.3402603233408159622 ) ) ;
#8059 = CARTESIAN_POINT ( 'NONE',  ( 0.2230971623002954429, 0.2230971623002953319, 0.2081250000000026412 ) ) ;
#8060 = DIRECTION ( 'NONE',  ( -0.5773502691896257311, -0.5773502691896257311, -0.5773502691896257311 ) ) ;
#8061 = CARTESIAN_POINT ( 'NONE',  ( -0.2688584691416579520, -0.07459580784763643335, -0.06776396657361484499 ) ) ;
#8062 = CARTESIAN_POINT ( 'NONE',  ( -5.178964085587577574E-17, 0.4659722221463555858, 0.2819296736111110979 ) ) ;
#8063 = CARTESIAN_POINT ( 'NONE',  ( 0.1993543840281266910, 0.2090277777019111383, -0.1993543840281266910 ) ) ;
#8064 = CARTESIAN_POINT ( 'NONE',  ( -0.2819296736111110424, 4.203555555631421470, 0.1167790944451424923 ) ) ;
#8065 = CARTESIAN_POINT ( 'NONE',  ( -0.1236067977499789583, 0.3410714283763437993, -0.3804226065180614791 ) ) ;
#8066 = CARTESIAN_POINT ( 'NONE',  ( 0.2819296736111110424, 4.842444444520309865, -0.1167790944451423396 ) ) ;
#8067 = DIRECTION ( 'NONE',  ( -0.000000000000000000, -1.000000000000000000, -0.000000000000000000 ) ) ;
#8068 = CIRCLE ( 'NONE', #3793, 0.3125000000000000000 ) ;
#8069 = CARTESIAN_POINT ( 'NONE',  ( 0.1292346314604058410, 3.963972222373954413, 0.3119999999999998885 ) ) ;
#8070 = CARTESIAN_POINT ( 'NONE',  ( 0.2085087158397508078, -0.1823754829288359303, 0.3880822748423157220 ) ) ;
#8071 =( LENGTH_UNIT ( ) NAMED_UNIT ( * ) SI_UNIT ( $, .METRE. ) );
#8072 = VERTEX_POINT ( 'NONE', #2847 ) ;
#8073 = MECHANICAL_CONTEXT ( 'NONE', #1723, 'mechanical' ) ;
#8074 = DIRECTION ( 'NONE',  ( -0.000000000000000000, 1.000000000000000000, -0.000000000000000000 ) ) ;
#8075 = CARTESIAN_POINT ( 'NONE',  ( -0.4366234456863258839, 1.999640111863030478, -2.684082427924094016 ) ) ;
#8076 = ORIENTED_EDGE ( 'NONE', *, *, #20394, .T. ) ;
#8077 = CARTESIAN_POINT ( 'NONE',  ( 0.2819296736111110424, 0.05277777770191114520, -0.1167790944451423119 ) ) ;
#8078 = AXIS2_PLACEMENT_3D ( 'NONE', #18966, #302, #9338 ) ;
#8079 = ORIENTED_EDGE ( 'NONE', *, *, #18910, .T. ) ;
#8080 = CARTESIAN_POINT ( 'NONE',  ( 0.006132810802118407977, 4.265890496703536705, -0.3119484895688790504 ) ) ;
#8081 = CARTESIAN_POINT ( 'NONE',  ( 0.2142276530138180479, 0.4175814842298848917, 0.4181133580835095231 ) ) ;
#8082 = CARTESIAN_POINT ( 'NONE',  ( 0.0007409178576027871874, 4.766034521252337619, -0.3119991761991793844 ) ) ;
#8083 = CARTESIAN_POINT ( 'NONE',  ( -0.2923287055106771337, 0.3223214284738861735, 0.2123892367102619971 ) ) ;
#8084 = CARTESIAN_POINT ( 'NONE',  ( 4.312521114635084752E-13, 5.190332509204934830, -0.2890970118899086061 ) ) ;
#8085 = VERTEX_POINT ( 'NONE', #8696 ) ;
#8086 = CARTESIAN_POINT ( 'NONE',  ( -0.1116596296178199582, 0.3187499999024575592, -0.3436530038418508792 ) ) ;
#8087 = CARTESIAN_POINT ( 'NONE',  ( -0.2648504260907811325, 4.673840770439461778, 0.1658194286430906550 ) ) ;
#8088 = CARTESIAN_POINT ( 'NONE',  ( 0.2819296736111110979, 4.047305555631421470, -3.452642723725051716E-17 ) ) ;
#8089 = CARTESIAN_POINT ( 'NONE',  ( -0.4593750000000003664, -0.2760455974562901482, 0.3779506566538943235 ) ) ;
#8090 = CARTESIAN_POINT ( 'NONE',  ( -0.1463856370309246369, 5.168083914757449548, -0.2593197864242284822 ) ) ;
#8091 =( REPRESENTATION_RELATIONSHIP ('NONE','NONE', #4490, #4350 ) REPRESENTATION_RELATIONSHIP_WITH_TRANSFORMATION ( #1968 )SHAPE_REPRESENTATION_RELATIONSHIP( ) );
#8092 = EDGE_CURVE ( 'NONE', #19908, #16571, #17089, .T. ) ;
#8093 = CARTESIAN_POINT ( 'NONE',  ( 0.3119999999999999996, 4.418833333485065573, -3.820898013339742174E-17 ) ) ;
#8094 = CARTESIAN_POINT ( 'NONE',  ( 0.2819296736111111534, 5.002166666742533074, 0.1167790944451422563 ) ) ;
#8095 = ORIENTED_EDGE ( 'NONE', *, *, #15927, .T. ) ;
#8096 = CARTESIAN_POINT ( 'NONE',  ( -1.726321361862525858E-17, 4.116750000075865223, -0.2819296736111110979 ) ) ;
#8097 = VERTEX_POINT ( 'NONE', #16866 ) ;
#8098 = ADVANCED_FACE ( 'NONE', ( #22471 ), #5824, .T. ) ;
#8099 = ORIENTED_EDGE ( 'NONE', *, *, #19005, .T. ) ;
#8100 = ORIENTED_EDGE ( 'NONE', *, *, #3010, .F. ) ;
#8101 = CALENDAR_DATE ( 2026, 7, 10 ) ;
#8102 = CARTESIAN_POINT ( 'NONE',  ( 0.4683334081279746930, 0.2655573993979199465, 0.04698409998688510975 ) ) ;
#8103 = CARTESIAN_POINT ( 'NONE',  ( 0.3125000000000000000, -5.740531871003217465E-17, 0.2550000000000030020 ) ) ;
#8104 = CARTESIAN_POINT ( 'NONE',  ( 1.910449006669871087E-17, 0.08055555540382261515, -0.3119999999999999996 ) ) ;
#8105 = CARTESIAN_POINT ( 'NONE',  ( 0.2323269574505744950, 4.412370849970273845, 0.2096127310370168306 ) ) ;
#8106 = CARTESIAN_POINT ( 'NONE',  ( -0.4687500000000004441, -0.08803459774007682537, 0.4135153894406012887 ) ) ;
#8107 = CARTESIAN_POINT ( 'NONE',  ( 0.4620259694561524855, -0.2880908832651559170, 0.04413116910601655452 ) ) ;
#8108 = VECTOR ( 'NONE', #22325, 39.37007874015748854 ) ;
#8109 = CARTESIAN_POINT ( 'NONE',  ( -0.2764156081756484196, 0.1144950937579609918, 0.2515277777777809587 ) ) ;
#8110 = CARTESIAN_POINT ( 'NONE',  ( 1.726321361862525858E-17, 0.4520833332574667462, -0.2819296736111110979 ) ) ;
#8111 = CARTESIAN_POINT ( 'NONE',  ( -0.2764156081756484196, 1.692557448933383907E-17, 0.4286111111111156613 ) ) ;
#8112 = ORIENTED_EDGE ( 'NONE', *, *, #6373, .T. ) ;
#8113 = CARTESIAN_POINT ( 'NONE',  ( 0.1167790944451424368, 4.717444444520309865, 0.2819296736111110424 ) ) ;
#8114 = CARTESIAN_POINT ( 'NONE',  ( -0.1166234456863257940, 1.999640111863030478, -2.802594437230252922 ) ) ;
#8115 = CARTESIAN_POINT ( 'NONE',  ( -0.1167790944451423535, 4.752166666742533074, 0.2819296736111110424 ) ) ;
#8116 = CARTESIAN_POINT ( 'NONE',  ( -0.04059609524757908788, 4.156104316328405268, -0.3095148733534341390 ) ) ;
#8117 = EDGE_CURVE ( 'NONE', #1934, #2014, #22913, .T. ) ;
#8118 = EDGE_CURVE ( 'NONE', #4381, #22719, #20587, .T. ) ;
#8119 = CARTESIAN_POINT ( 'NONE',  ( 0.2967211878843482586, 4.860212748769966673, 0.1045282615683273547 ) ) ;
#8120 = DIRECTION ( 'NONE',  ( -0.000000000000000000, -1.000000000000000000, -0.000000000000000000 ) ) ;
#8121 = FACE_OUTER_BOUND ( 'NONE', #14655, .T. ) ;
#8122 = ADVANCED_FACE ( 'NONE', ( #10906 ), #12870, .T. ) ;
#8123 = CARTESIAN_POINT ( 'NONE',  ( 0.3119999999999999996, 4.352861111111110404, 0.1292346314604056190 ) ) ;
#8124 = EDGE_CURVE ( 'NONE', #5262, #5711, #2336, .T. ) ;
#8125 = CARTESIAN_POINT ( 'NONE',  ( -0.3125000000000000000, 1.913510623667739771E-17, 0.1716666666666689933 ) ) ;
#8126 = CARTESIAN_POINT ( 'NONE',  ( -0.1292346314604058410, 0.5493055554038226429, 0.3119999999999998885 ) ) ;
#8127 = EDGE_LOOP ( 'NONE', ( #14298, #12029, #2106, #18952 ) ) ;
#8128 = CARTESIAN_POINT ( 'NONE',  ( 0.2672908904913715578, 4.580718530736621830, 0.1620962247036812631 ) ) ;
#8129 = ORIENTED_EDGE ( 'NONE', *, *, #14863, .T. ) ;
#8130 = ADVANCED_FACE ( 'NONE', ( #9064 ), #6492, .F. ) ;
#8131 = DIRECTION ( 'NONE',  ( -0.000000000000000000, -1.000000000000000000, -0.000000000000000000 ) ) ;
#8132 = AXIS2_PLACEMENT_3D ( 'NONE', #21172, #10783, #1504 ) ;
#8133 = CARTESIAN_POINT ( 'NONE',  ( 0.3105407428941047709, 4.142119987277710358, -0.03873399703425771390 ) ) ;
#8134 = CARTESIAN_POINT ( 'NONE',  ( 0.1306872919485614071, -0.3155070326520293955, -0.1390972222222219556 ) ) ;
#8135 = ADVANCED_FACE ( 'NONE', ( #11382 ), #22708, .F. ) ;
#8136 = CARTESIAN_POINT ( 'NONE',  ( -0.02550062582863994037, 3.933446043089724231, -0.3109980386088752047 ) ) ;
#8137 = ORIENTED_EDGE ( 'NONE', *, *, #16678, .T. ) ;
#8138 = CARTESIAN_POINT ( 'NONE',  ( 0.2233192592356399164, 0.05446428561674330343, 0.3073725909049500604 ) ) ;
#8139 = CARTESIAN_POINT ( 'NONE',  ( 1.726321361862525858E-17, 0.4381944443685778512, -0.2819296736111110979 ) ) ;
#8140 = SPHERICAL_SURFACE ( 'NONE', #12904, 0.3119999999999999996 ) ;
#8141 = DIRECTION ( 'NONE',  ( -0.8660254037844382635, 0.000000000000000000, 0.5000000000000004441 ) ) ;
#8142 = FACE_OUTER_BOUND ( 'NONE', #11125, .T. ) ;
#8143 = CARTESIAN_POINT ( 'NONE',  ( 0.2764156081756483641, 0.1144950937579610056, 0.2931944444444479214 ) ) ;
#8144 = VERTEX_POINT ( 'NONE', #23058 ) ;
#8145 = CARTESIAN_POINT ( 'NONE',  ( 0.000000000000000000, 0.8699999999999998845, 0.000000000000000000 ) ) ;
#8146 = FACE_OUTER_BOUND ( 'NONE', #9450, .T. ) ;
#8147 = CARTESIAN_POINT ( 'NONE',  ( 0.1690789815138871444, -4.088425335522419233E-18, -0.3319522695443154481 ) ) ;
#8148 = CARTESIAN_POINT ( 'NONE',  ( -5.731347020009612645E-17, 0.3374999999999996336, 0.3119999999999999996 ) ) ;
#8149 = CARTESIAN_POINT ( 'NONE',  ( -0.3119999999999999996, 4.884111111111110404, 0.000000000000000000 ) ) ;
#8150 = AXIS2_PLACEMENT_3D ( 'NONE', #5214, #22289, #12935 ) ;
#8151 = CARTESIAN_POINT ( 'NONE',  ( -0.2819296736111110979, 3.977861111186976828, 0.000000000000000000 ) ) ;
#8152 = DIRECTION ( 'NONE',  ( 0.7071067811865475727, 0.000000000000000000, 0.7071067811865474617 ) ) ;
#8153 = CARTESIAN_POINT ( 'NONE',  ( -0.2206173157302027676, 3.891055555555554601, 0.2206173157302028787 ) ) ;
#8154 = DIRECTION ( 'NONE',  ( -1.000000000000000000, 0.000000000000000000, 0.000000000000000000 ) ) ;
#8155 = ORIENTED_EDGE ( 'NONE', *, *, #19743, .F. ) ;
#8156 = CARTESIAN_POINT ( 'NONE',  ( -0.3119999973396838655, 4.001073216847850667, -0.04084072313200213383 ) ) ;
#8157 = EDGE_CURVE ( 'NONE', #5331, #4062, #8986, .T. ) ;
#8158 = CARTESIAN_POINT ( 'NONE',  ( 0.1167790944451422702, 4.779944444520309865, -0.2819296736111110424 ) ) ;
#8159 = EDGE_CURVE ( 'NONE', #23837, #3289, #3216, .T. ) ;
#8160 = CARTESIAN_POINT ( 'NONE',  ( 0.09145417301143894673, -0.5014751291207466544, 0.06110928887248360392 ) ) ;
#8161 = CARTESIAN_POINT ( 'NONE',  ( 0.1578986201652094745, -0.4501030665082204063, 0.4142710792078265758 ) ) ;
#8162 = CARTESIAN_POINT ( 'NONE',  ( 3.820898013339742174E-17, 5.384999999999999787, 0.3119999999999999996 ) ) ;
#8163 = VECTOR ( 'NONE', #16933, 39.37007874015748143 ) ;
#8164 = CARTESIAN_POINT ( 'NONE',  ( 0.4687500000000002776, -0.2598076211353317344, 0.4425000000000000044 ) ) ;
#8165 = VECTOR ( 'NONE', #1183, 39.37007874015748143 ) ;
#8166 = CARTESIAN_POINT ( 'NONE',  ( -0.1993543840281266910, 4.248694444520310753, -0.1993543840281266910 ) ) ;
#8167 = CARTESIAN_POINT ( 'NONE',  ( -0.06581070416570369841, 4.045665677644000091, -0.3054227462770962020 ) ) ;
#8168 = CARTESIAN_POINT ( 'NONE',  ( 1.573500000000000121, 0.6376613660676677675, -0.3524999999999999800 ) ) ;
#8169 = FACE_OUTER_BOUND ( 'NONE', #8727, .T. ) ;
#8170 = CARTESIAN_POINT ( 'NONE',  ( -5.178964085587577574E-17, 0.4243055554796889006, 0.2819296736111110979 ) ) ;
#8171 = LINE ( 'NONE', #982, #23216 ) ;
#8172 = CARTESIAN_POINT ( 'NONE',  ( -4.638126268221291196E-16, 0.1321428571428571175, -0.4000000000000000222 ) ) ;
#8173 = CARTESIAN_POINT ( 'NONE',  ( 0.3999999999999999667, 0.3321428571428570731, -0.1299678784931625475 ) ) ;
#8174 = CARTESIAN_POINT ( 'NONE',  ( 0.2230971623002953874, -0.2230971623002954429, 0.2497916666666696317 ) ) ;
#8175 = DIRECTION ( 'NONE',  ( 1.000000000000000000, 0.000000000000000000, 1.224646799147353207E-16 ) ) ;
#8176 = CARTESIAN_POINT ( 'NONE',  ( -0.1917236326748512631, 3.771781958134273083, -0.2495076210021671681 ) ) ;
#8177 = CARTESIAN_POINT ( 'NONE',  ( -0.1993543840281266633, 0.5006944443685777957, -0.1993543840281266910 ) ) ;
#8178 = CARTESIAN_POINT ( 'NONE',  ( 0.2819296736111110424, 0.2055555554796889006, -0.1167790944451423119 ) ) ;
#8179 = CARTESIAN_POINT ( 'NONE',  ( 0.1993543840281266633, 3.957027777853643791, -0.1993543840281266910 ) ) ;
#8180 = CARTESIAN_POINT ( 'NONE',  ( 0.3236067977499790249, 0.2553571426620580009, -0.2351141009169892826 ) ) ;
#8181 = CARTESIAN_POINT ( 'NONE',  ( -0.2819296736111110424, 4.696611111186977716, -0.1167790944451423119 ) ) ;
#8182 = CONICAL_SURFACE ( 'NONE', #12119, 0.3308333333333332571, 0.7853981633974427279 ) ;
#8183 = CARTESIAN_POINT ( 'NONE',  ( 0.3029461644517479901, 5.080632737976908508, -0.07557799413177579417 ) ) ;
#8184 = VECTOR ( 'NONE', #21677, 39.37007874015748143 ) ;
#8185 = ORIENTED_EDGE ( 'NONE', *, *, #20654, .T. ) ;
#8186 = ORIENTED_EDGE ( 'NONE', *, *, #18271, .F. ) ;
#8187 = CARTESIAN_POINT ( 'NONE',  ( -0.1294417382415922191, 0.3125000000000000000, 0.1056944444444462838 ) ) ;
#8188 = CARTESIAN_POINT ( 'NONE',  ( 0.3119999999999999996, 3.811194444596177622, -0.1292346314604056745 ) ) ;
#8189 = CARTESIAN_POINT ( 'NONE',  ( 0.1229229017544715696, -0.2477443904640376227, 0.3880822748423153334 ) ) ;
#8190 =( BOUNDED_CURVE ( )  B_SPLINE_CURVE ( 2, ( #12376, #10778, #18204, #14551, #18322, #11016, #8229, #1500, #1620 ),
 .UNSPECIFIED., .F., .T. ) 
 B_SPLINE_CURVE_WITH_KNOTS ( ( 3, 2, 2, 2, 3 ),
 ( 0.9553571428571425717, 0.9598214285714283811, 0.9642857142857141906, 0.9687500000000000000, 0.9732142857142858094 ),
 .UNSPECIFIED. ) 
 CURVE ( )  GEOMETRIC_REPRESENTATION_ITEM ( )  RATIONAL_B_SPLINE_CURVE ( ( 1.000000000000005773, 0.9238795325112810763, 1.000000000000000000, 0.9238795325112867385, 1.000000000000000000, 0.9238795325112867385, 1.000000000000000000, 0.9238795325112848511, 1.000000000000001998 ) ) 
 REPRESENTATION_ITEM ( '' )  );
#8191 =( NAMED_UNIT ( * ) SI_UNIT ( $, .STERADIAN. ) SOLID_ANGLE_UNIT ( ) );
#8192 = ORIENTED_EDGE ( 'NONE', *, *, #10311, .T. ) ;
#8193 =( BOUNDED_SURFACE ( )  B_SPLINE_SURFACE ( 2, 3, ( 
 ( #1015, #15890, #17846, #4910, #23310, #14068, #1137, #8572, #16013, #23431 ),
 ( #21616, #7229, #19911, #12611, #3559, #12855, #12490, #6987, #11129, #3200 ),
 ( #20029, #5144, #18078, #1378, #5390, #8807, #18201, #14675, #20272, #1497 ) ),
 .UNSPECIFIED., .F., .F., .T. ) 
 B_SPLINE_SURFACE_WITH_KNOTS ( ( 3, 3 ),
 ( 4, 3, 3, 4 ),
 ( 0.000000000000000000, 1.000000000000000000 ),
 ( 0.01132290749860157507, 0.02432858112762278230, 0.08935694927272853916, 0.1023626229017496891 ),
 .UNSPECIFIED. ) 
 GEOMETRIC_REPRESENTATION_ITEM ( )  RATIONAL_B_SPLINE_SURFACE ( (
 ( 1.000000000000000000, 1.000000000000000000, 1.000000000000000000, 1.000000000000000000, 1.000000000000000000, 1.000000000000000000, 1.000000000000000000, 1.000000000000000000, 1.000000000000000000, 1.000000000000000000),
 ( 0.4999999999999997780, 0.4999999999999997780, 0.4999999999999997780, 0.4999999999999997780, 0.4999999999999997780, 0.4999999999999997780, 0.4999999999999997780, 0.4999999999999997780, 0.4999999999999997780, 0.4999999999999997780),
 ( 1.000000000000000000, 1.000000000000000000, 1.000000000000000000, 1.000000000000000000, 1.000000000000000000, 1.000000000000000000, 1.000000000000000000, 1.000000000000000000, 1.000000000000000000, 1.000000000000000000) ) ) 
 REPRESENTATION_ITEM ( '' )  SURFACE ( )  );
#8194 = COORDINATED_UNIVERSAL_TIME_OFFSET ( 0, 0, .AHEAD. ) ;
#8195 = ORIENTED_EDGE ( 'NONE', *, *, #23305, .T. ) ;
#8196 = CARTESIAN_POINT ( 'NONE',  ( 0.3999999999999999667, 0.4589285712334865708, 0.1299678784931626307 ) ) ;
#8197 = AXIS2_PLACEMENT_3D ( 'NONE', #15806, #10211, #4703 ) ;
#8198 = CARTESIAN_POINT ( 'NONE',  ( -0.4416234456863259439, 1.828961980248579033, -2.681195676578145726 ) ) ;
#8199 = ORIENTED_EDGE ( 'NONE', *, *, #17960, .T. ) ;
#8200 = CARTESIAN_POINT ( 'NONE',  ( 0.2819296736111110979, 0.1048611110352444808, 0.000000000000000000 ) ) ;
#8201 = AXIS2_PLACEMENT_3D ( 'NONE', #13319, #4033, #8049 ) ;
#8202 = CARTESIAN_POINT ( 'NONE',  ( 0.003049558294924298047, 4.265973550867800057, -0.3119872481712610002 ) ) ;
#8203 = CARTESIAN_POINT ( 'NONE',  ( 0.04282247326130569909, 0.5165423109005278235, 0.4011144384304308752 ) ) ;
#8204 = CARTESIAN_POINT ( 'NONE',  ( 0.2576415818302536520, 4.080194459578224020, 0.1799301507806963518 ) ) ;
#8205 = CARTESIAN_POINT ( 'NONE',  ( 0.1116596296178199860, 0.2223214284738861402, -0.3436530038418508792 ) ) ;
#8206 = CARTESIAN_POINT ( 'NONE',  ( 0.1933203555740233281, 5.172664093799754781, 0.2239000762248374854 ) ) ;
#8207 = CARTESIAN_POINT ( 'NONE',  ( -1.910449006669871087E-17, 4.092444444444444329, -0.3119999999999999996 ) ) ;
#8208 = CARTESIAN_POINT ( 'NONE',  ( -0.09135502326330770251, -0.5015332108058754290, 0.06108558933789662304 ) ) ;
#8209 = APPROVAL ( #18429, 'UNKNOWN' ) ;
#8210 = CARTESIAN_POINT ( 'NONE',  ( -0.2819296736111110424, 4.078555555631421470, 0.1167790944451424923 ) ) ;
#8211 = CARTESIAN_POINT ( 'NONE',  ( -0.1292346314604058410, 0.1048611109593781676, 0.3119999999999998885 ) ) ;
#8212 = CARTESIAN_POINT ( 'NONE',  ( -0.2332192335059636024, 5.186968840224980504, 0.1733688601932164841 ) ) ;
#8213 = CARTESIAN_POINT ( 'NONE',  ( 3.820898013339742174E-17, 5.384999999999999787, 0.3119999999999999996 ) ) ;
#8214 = CARTESIAN_POINT ( 'NONE',  ( 5.731347020009612645E-17, 4.516055555707287894, 0.3119999999999999996 ) ) ;
#8215 = CARTESIAN_POINT ( 'NONE',  ( 0.2819296736111110979, 5.009111111186976828, -0.1167790944451423396 ) ) ;
#8216 = AXIS2_PLACEMENT_3D ( 'NONE', #10732, #16821, #20354 ) ;
#8217 = CARTESIAN_POINT ( 'NONE',  ( -0.2819296736111110424, 4.078555555631421470, 0.1167790944451424923 ) ) ;
#8218 = CARTESIAN_POINT ( 'NONE',  ( 0.1116596296178199027, 0.2651785713310289561, 0.3436530038418508792 ) ) ;
#8219 = ORIENTED_EDGE ( 'NONE', *, *, #22918, .T. ) ;
#8220 = VERTEX_POINT ( 'NONE', #9549 ) ;
#8221 = B_SPLINE_CURVE_WITH_KNOTS ( 'NONE', 3,
 ( #8556, #6368, #23179, #11880, #4296, #8189, #19294, #21252, #2598, #4539, #8070, #10408 ),
 .UNSPECIFIED., .F., .F.,
 ( 4, 2, 2, 2, 2, 4 ),
 ( 5.846333392818911776E-17, 0.001386135995484567536, 0.002079203993226821489, 0.002772271990969075225, 0.004158407986453582263, 0.005544543981938090602 ),
 .UNSPECIFIED. ) ;
#8222 = PERSON_AND_ORGANIZATION_ROLE ( 'classification_officer' ) ;
#8223 = CARTESIAN_POINT ( 'NONE',  ( -0.2111984196243033851, -0.4085062965502692101, 0.4344098397133764333 ) ) ;
#8224 = CARTESIAN_POINT ( 'NONE',  ( -0.2209708691207961095, 0.2209708691207961373, 0.2758333333333364834 ) ) ;
#8225 = CARTESIAN_POINT ( 'NONE',  ( 0.4584515285649273242, 0.2213539724899254713, 0.4064761396644160363 ) ) ;
#8226 = CARTESIAN_POINT ( 'NONE',  ( -1.960390272410463459E-06, 4.210500054279665783, -0.3119999999938410928 ) ) ;
#8227 = CARTESIAN_POINT ( 'NONE',  ( 0.3119999999999999996, 0.1812499998482670904, -0.1292346314604056468 ) ) ;
#8228 = CARTESIAN_POINT ( 'NONE',  ( -0.3125000000000000000, 1.913510623667739771E-17, -0.09916666666666609786 ) ) ;
#8229 = CARTESIAN_POINT ( 'NONE',  ( -0.2206173157302028232, 3.766055555555554601, -0.2206173157302028232 ) ) ;
#8230 = ORIENTED_EDGE ( 'NONE', *, *, #6335, .T. ) ;
#8231 = LINE ( 'NONE', #21651, #23185 ) ;
#8232 = CARTESIAN_POINT ( 'NONE',  ( 0.000000000000000000, 0.4199999999999998734, 0.000000000000000000 ) ) ;
#8233 = CARTESIAN_POINT ( 'NONE',  ( 0.2764156081756483641, -0.1144950937579611167, 0.1681944444444469777 ) ) ;
#8234 = LINE ( 'NONE', #11926, #22168 ) ;
#8235 = ADVANCED_FACE ( 'NONE', ( #15401 ), #13705, .T. ) ;
#8236 = CARTESIAN_POINT ( 'NONE',  ( 0.1167790944451424368, 4.703555555631420582, 0.2819296736111110424 ) ) ;
#8237 = CARTESIAN_POINT ( 'NONE',  ( 0.4587493717650694691, -0.1772960527124521901, 0.4158887382153850787 ) ) ;
#8238 = DIRECTION ( 'NONE',  ( 0.9063077870366478273, 1.109906930436751740E-16, -0.4226182617407038267 ) ) ;
#8239 = CARTESIAN_POINT ( 'NONE',  ( -0.01610145506848609243, 4.708926481085645203E-18, 0.3730084384222186467 ) ) ;
#8240 = PLANE ( 'NONE',  #17802 ) ;
#8241 = CARTESIAN_POINT ( 'NONE',  ( -0.1292346314604056745, 4.318138888888888083, -0.3119999999999999996 ) ) ;
#8242 = FACE_OUTER_BOUND ( 'NONE', #947, .T. ) ;
#8243 = FACE_OUTER_BOUND ( 'NONE', #9596, .T. ) ;
#8244 = CARTESIAN_POINT ( 'NONE',  ( 0.08226311336655546536, 4.962829471254590175, 0.3009951623300980428 ) ) ;
#8245 = ADVANCED_BREP_SHAPE_REPRESENTATION ( '', ( #8780, #9127 ), #14988 ) ;
#8246 = LINE ( 'NONE', #23113, #1804 ) ;
#8247 = VERTEX_POINT ( 'NONE', #15162 ) ;
#8248 = B_SPLINE_CURVE_WITH_KNOTS ( 'NONE', 1,
 ( #12129, #8560 ),
 .UNSPECIFIED., .F., .F.,
 ( 2, 2 ),
 ( 0.000000000000000000, 1.000000000000000000 ),
 .UNSPECIFIED. ) ;
#8249 = DIRECTION ( 'NONE',  ( 0.5773502691896257311, -0.5773502691896257311, 0.5773502691896257311 ) ) ;
#8250 = VERTEX_POINT ( 'NONE', #22830 ) ;
#8251 = CARTESIAN_POINT ( 'NONE',  ( 0.2833369697430000445, 4.700439859952622257, -0.1306314325063157311 ) ) ;
#8252 = CARTESIAN_POINT ( 'NONE',  ( 0.1907739469436010582, 4.133017026477499911, 0.2468791227802183130 ) ) ;
#8253 = CARTESIAN_POINT ( 'NONE',  ( 0.1306872919485614071, -0.3155070326520293955, 0.1386805555555580272 ) ) ;
#8254 = EDGE_CURVE ( 'NONE', #16767, #12181, #2443, .T. ) ;
#8255 = EDGE_CURVE ( 'NONE', #6883, #6320, #17345, .T. ) ;
#8256 = VECTOR ( 'NONE', #9301, 39.37007874015748854 ) ;
#8257 = CARTESIAN_POINT ( 'NONE',  ( -0.1586475693114280106, -0.4496706605170417981, 0.08858850926231189027 ) ) ;
#8258 = CARTESIAN_POINT ( 'NONE',  ( -0.1116596296178199582, -0.05625000009754239222, -0.3436530038418508792 ) ) ;
#8259 = CARTESIAN_POINT ( 'NONE',  ( -0.2819296736111110979, 0.07361111103524446697, -0.1167790944451423396 ) ) ;
#8260 = CARTESIAN_POINT ( 'NONE',  ( -0.09561951185436078082, 5.206640035683668621, 0.2653980274966651343 ) ) ;
#8261 = LINE ( 'NONE', #4721, #3012 ) ;
#8262 = CARTESIAN_POINT ( 'NONE',  ( 0.1292346314604057300, 0.5076388888888885287, 0.3119999999999998885 ) ) ;
#8263 = CARTESIAN_POINT ( 'NONE',  ( -0.2764156081756484196, 0.1144950937579609918, 0.3140277777777814583 ) ) ;
#8264 = EDGE_CURVE ( 'NONE', #19381, #9492, #13339, .T. ) ;
#8265 = VERTEX_POINT ( 'NONE', #20761 ) ;
#8266 = CARTESIAN_POINT ( 'NONE',  ( 0.000000000000000000, 6.000000000000000888, 0.000000000000000000 ) ) ;
#8267 = CARTESIAN_POINT ( 'NONE',  ( 0.000000000000000000, 5.384999999999999787, -0.3119999999999999996 ) ) ;
#8268 = CARTESIAN_POINT ( 'NONE',  ( 0.3119999999999999996, 4.748694444444444329, -0.1292346314604056745 ) ) ;
#8269 = CARTESIAN_POINT ( 'NONE',  ( 0.2206173157302027676, 0.5666666666666663188, 0.2206173157302028787 ) ) ;
#8270 = CARTESIAN_POINT ( 'NONE',  ( -0.2206173157302027676, 5.057722222222222008, 0.2206173157302028787 ) ) ;
#8271 = CARTESIAN_POINT ( 'NONE',  ( 0.1993543840281266633, 4.068138888964754507, -0.1993543840281266910 ) ) ;
#8272 = DIRECTION ( 'NONE',  ( 0.5000000000000007772, 0.000000000000000000, 0.8660254037844382635 ) ) ;
#8273 = DIRECTION ( 'NONE',  ( -0.000000000000000000, -0.9607689228305225093, 0.2773500981126159615 ) ) ;
#8274 = CARTESIAN_POINT ( 'NONE',  ( 0.3380520187481464989, 3.229549314084639149E-17, 0.1297593444830981713 ) ) ;
#8275 = ORIENTED_EDGE ( 'NONE', *, *, #14455, .F. ) ;
#8276 = VERTEX_POINT ( 'NONE', #4052 ) ;
#8277 = CARTESIAN_POINT ( 'NONE',  ( -0.1917386021594863765, 4.010339725230847030, 0.2494960349349919226 ) ) ;
#8278 = CARTESIAN_POINT ( 'NONE',  ( -0.2819296736111110424, 4.682722222298087544, -0.1167790944451423119 ) ) ;
#8279 = VECTOR ( 'NONE', #15400, 39.37007874015748854 ) ;
#8280 = CARTESIAN_POINT ( 'NONE',  ( -0.3613381517857143788, 0.3187499999024575592, 0.1174058825155740310 ) ) ;
#8281 = PERSON_AND_ORGANIZATION_ROLE ( 'creator' ) ;
#8282 = CARTESIAN_POINT ( 'NONE',  ( 0.4450000000000002842, 0.000000000000000000, -1.879397459621555244 ) ) ;
#8283 = CARTESIAN_POINT ( 'NONE',  ( -0.1144950937579609918, -0.2764156081756484196, 0.09875000000000196121 ) ) ;
#8284 = EDGE_CURVE ( 'NONE', #11232, #14303, #18942, .T. ) ;
#8285 = CARTESIAN_POINT ( 'NONE',  ( 0.1993543840281267465, 4.332027777853642903, 0.1993543840281266633 ) ) ;
#8286 = APPROVAL_DATE_TIME ( #6699, #19998 ) ;
#8287 = CARTESIAN_POINT ( 'NONE',  ( 0.3830434977118160611, -0.3085929194348117632, 0.4166771511014250029 ) ) ;
#8288 = CARTESIAN_POINT ( 'NONE',  ( 0.3125000000000000000, -5.740531871003217465E-17, 0.3105555555555590819 ) ) ;
#8289 = CARTESIAN_POINT ( 'NONE',  ( -0.1954553509668046640, 0.1954553509668046918, 0.3105555555555591929 ) ) ;
#8290 = CARTESIAN_POINT ( 'NONE',  ( 0.5550849365154918447, 2.740000000000000213, -0.7321440192514540035 ) ) ;
#8291 = CARTESIAN_POINT ( 'NONE',  ( -0.1167790944451422702, -0.002777777853644409437, -0.2819296736111110424 ) ) ;
#8292 = DIRECTION ( 'NONE',  ( -0.5773502691896256200, 0.5773502691896194028, -0.5773502691896320593 ) ) ;
#8293 = CARTESIAN_POINT ( 'NONE',  ( 0.000000000000000000, 5.384999999999999787, -0.3119999999999999996 ) ) ;
#8294 = CARTESIAN_POINT ( 'NONE',  ( -0.1294417382415922191, 0.3125000000000000000, -0.005416666666665734438 ) ) ;
#8295 = CARTESIAN_POINT ( 'NONE',  ( -0.3155070326520292845, 1.931923388228935888E-17, 0.2845138888888921191 ) ) ;
#8296 = VECTOR ( 'NONE', #8989, 39.37007874015748854 ) ;
#8297 = EDGE_CURVE ( 'NONE', #412, #428, #17131, .T. ) ;
#8298 = DIRECTION ( 'NONE',  ( -1.000000000000000000, 0.000000000000000000, 0.000000000000000000 ) ) ;
#8299 = LINE ( 'NONE', #19520, #21036 ) ;
#8300 = CARTESIAN_POINT ( 'NONE',  ( -0.1167790944451422702, 0.3861111110352444808, -0.2819296736111110979 ) ) ;
#8301 = CARTESIAN_POINT ( 'NONE',  ( 0.2819296736111110424, 0.5388888888130223265, -0.1167790944451423119 ) ) ;
#8302 = CARTESIAN_POINT ( 'NONE',  ( 0.2819296736111110424, 4.009111111186976828, -0.1167790944451423396 ) ) ;
#8303 = CARTESIAN_POINT ( 'NONE',  ( -0.3236067977499789694, 0.3482142855192008613, -0.2351141009169893104 ) ) ;
#8304 = CARTESIAN_POINT ( 'NONE',  ( 5.178964085587577574E-17, 4.658416666742532186, 0.2819296736111110979 ) ) ;
#8305 = LINE ( 'NONE', #3728, #17438 ) ;
#8306 = CARTESIAN_POINT ( 'NONE',  ( 0.3029724772689905699, 5.076302895770250068, 0.07975337583219681281 ) ) ;
#8307 = ORIENTED_EDGE ( 'NONE', *, *, #2102, .T. ) ;
#8308 = ORIENTED_EDGE ( 'NONE', *, *, #16480, .F. ) ;
#8309 = CARTESIAN_POINT ( 'NONE',  ( 0.2206173157302028787, 4.793833333333332725, 0.2206173157302027954 ) ) ;
#8310 = CARTESIAN_POINT ( 'NONE',  ( 0.1292346314604056190, 3.873694444596177622, -0.3119999999999999996 ) ) ;
#8311 = CARTESIAN_POINT ( 'NONE',  ( 0.000000000000000000, 0.000000000000000000, 0.000000000000000000 ) ) ;
#8312 = CIRCLE ( 'NONE', #11449, 0.7500000000000001110 ) ;
#8313 = ORIENTED_EDGE ( 'NONE', *, *, #17163, .T. ) ;
#8314 = DATE_AND_TIME ( #883, #18146 ) ;
#8315 = VERTEX_POINT ( 'NONE', #4653 ) ;
#8316 = CARTESIAN_POINT ( 'NONE',  ( 3.025220084236446727, 2.291712385858714729, -2.986000000000001098 ) ) ;
#8317 = CARTESIAN_POINT ( 'NONE',  ( -0.05024295495402558709, 4.570215981136505512, 0.3079318380950444300 ) ) ;
#8318 = VERTEX_POINT ( 'NONE', #4767 ) ;
#8319 = CARTESIAN_POINT ( 'NONE',  ( 0.1292346314604057023, 0.6118055554038226429, 0.3119999999999998885 ) ) ;
#8320 = CARTESIAN_POINT ( 'NONE',  ( 0.2828977024960969144, 4.256026029941413213, -0.1315892272411629260 ) ) ;
#8321 = ADVANCED_FACE ( 'NONE', ( #14289 ), #8667, .T. ) ;
#8322 = CARTESIAN_POINT ( 'NONE',  ( -5.731347020009612645E-17, 0.3374999999999996336, 0.3119999999999999996 ) ) ;
#8323 = DIRECTION ( 'NONE',  ( 0.000000000000000000, 0.000000000000000000, 1.000000000000000000 ) ) ;
#8324 = CARTESIAN_POINT ( 'NONE',  ( -0.3613381517857143232, 0.2401785713310289894, -0.1174058825155741004 ) ) ;
#8325 = CARTESIAN_POINT ( 'NONE',  ( 0.04792230210257000106, 5.168523637897857625, 0.2932814512039932375 ) ) ;
#8326 = ADVANCED_FACE ( 'NONE', ( #10516 ), #14052, .T. ) ;
#8327 = CARTESIAN_POINT ( 'NONE',  ( -0.1116596296178200276, 0.2758928570453147433, 0.3436530038418508792 ) ) ;
#8328 = CARTESIAN_POINT ( 'NONE',  ( -0.2902337294436940773, 4.665514674916999560, -0.1145022281107502676 ) ) ;
#8329 = AXIS2_PLACEMENT_3D ( 'NONE', #21957, #7097, #14659 ) ;
#8330 = CARTESIAN_POINT ( 'NONE',  ( 0.1993543840281267465, 3.818138888964754507, 0.1993543840281266633 ) ) ;
#8331 = CARTESIAN_POINT ( 'NONE',  ( 0.05352015321003111142, 5.017547458390650306, 0.3073860041716943714 ) ) ;
#8332 = DIRECTION ( 'NONE',  ( 1.000000000000000000, 0.000000000000000000, 0.000000000000000000 ) ) ;
#8333 = CARTESIAN_POINT ( 'NONE',  ( 1.573500000000000343, 0.000000000000000000, -0.3524999999999999800 ) ) ;
#8334 = CARTESIAN_POINT ( 'NONE',  ( -0.2206173157302028232, 4.439666666818398610, -0.2206173157302028232 ) ) ;
#8335 = CARTESIAN_POINT ( 'NONE',  ( 0.1993543840281267465, 4.832027777853643791, 0.1993543840281266633 ) ) ;
#8336 = CARTESIAN_POINT ( 'NONE',  ( -0.2819296736111110979, 4.075083333409199149, 0.000000000000000000 ) ) ;
#8337 = ORIENTED_EDGE ( 'NONE', *, *, #10342, .F. ) ;
#8338 = ORIENTED_EDGE ( 'NONE', *, *, #23147, .T. ) ;
#8339 = DATE_AND_TIME ( #17620, #23560 ) ;
#8340 = ORIENTED_EDGE ( 'NONE', *, *, #13120, .T. ) ;
#8341 = CC_DESIGN_DATE_AND_TIME_ASSIGNMENT ( #12212, #2918, ( #22007 ) ) ;
#8342 = CARTESIAN_POINT ( 'NONE',  ( 0.3003475124358242487, 3.066692553488282957, 3.638968604327563749 ) ) ;
#8343 = CARTESIAN_POINT ( 'NONE',  ( -1.493307031895086562E-17, 0.4635611116728546865, -1.084197934689580034 ) ) ;
#8344 = CARTESIAN_POINT ( 'NONE',  ( 0.2726274893998235638, 0.3838643229717945138, 0.09139053646024344890 ) ) ;
#8345 = PLANE ( 'NONE',  #21420 ) ;
#8346 = CARTESIAN_POINT ( 'NONE',  ( 1.910449006669871087E-17, 0.1916666665149337478, -0.3119999999999999996 ) ) ;
#8347 = CARTESIAN_POINT ( 'NONE',  ( -0.3125000000000000000, -0.1294417382415921913, -0.09569444444444386022 ) ) ;
#8348 = AXIS2_PLACEMENT_3D ( 'NONE', #18311, #22203, #14787 ) ;
#8349 = CARTESIAN_POINT ( 'NONE',  ( -1.910449006669871087E-17, 4.147999999999998799, -0.3119999999999999996 ) ) ;
#8350 = DIRECTION ( 'NONE',  ( 0.000000000000000000, 0.000000000000000000, -1.000000000000000000 ) ) ;
#8351 = CARTESIAN_POINT ( 'NONE',  ( 0.1954553509668046640, -0.1954553509668047195, 0.05361111111111271227 ) ) ;
#8352 = ORIENTED_EDGE ( 'NONE', *, *, #17624, .F. ) ;
#8353 = CARTESIAN_POINT ( 'NONE',  ( -5.731347020009612645E-17, 0.5527777776260448528, 0.3119999999999999996 ) ) ;
#8354 = CARTESIAN_POINT ( 'NONE',  ( 0.1167790944451422702, 4.502166666742532186, -0.2819296736111110424 ) ) ;
#8355 = DIRECTION ( 'NONE',  ( 0.000000000000000000, 0.000000000000000000, -1.000000000000000000 ) ) ;
#8356 = CARTESIAN_POINT ( 'NONE',  ( 0.6391249999999999432, 7.864411439368920513E-17, 0.000000000000000000 ) ) ;
#8357 = DIRECTION ( 'NONE',  ( 0.000000000000000000, 0.000000000000000000, -1.000000000000000000 ) ) ;
#8358 = CARTESIAN_POINT ( 'NONE',  ( 6.614309848781084774E-13, 0.03242967361111062652, 0.2819296736111109869 ) ) ;
#8359 = CARTESIAN_POINT ( 'NONE',  ( -1.910449006669871087E-17, 4.259111111111110404, -0.3119999999999999996 ) ) ;
#8360 = CARTESIAN_POINT ( 'NONE',  ( 0.1294417382415924134, 0.3124999999999999445, 0.1543055555555577496 ) ) ;
#8361 = CARTESIAN_POINT ( 'NONE',  ( 0.3108823422949931192, 4.973667548811621764, 0.02638502853553916644 ) ) ;
#8362 = ORIENTED_EDGE ( 'NONE', *, *, #21874, .T. ) ;
#8363 = PRODUCT_DEFINITION_FORMATION_WITH_SPECIFIED_SOURCE ( 'ANY', '', #23325, .NOT_KNOWN. ) ;
#8364 = CARTESIAN_POINT ( 'NONE',  ( 0.3040647624429579921, 4.698881436987698557, -0.08103250758201478721 ) ) ;
#8365 = EDGE_CURVE ( 'NONE', #16517, #24032, #23653, .T. ) ;
#8366 = CARTESIAN_POINT ( 'NONE',  ( 0.3125000000000000000, 3.827021247335477694E-17, 1.326383476483184332 ) ) ;
#8367 = CARTESIAN_POINT ( 'NONE',  ( 0.000000000000000000, 0.3155070326520292845, 0.05187500000000178774 ) ) ;
#8368 = VECTOR ( 'NONE', #11090, 39.37007874015748854 ) ;
#8369 = CARTESIAN_POINT ( 'NONE',  ( 0.009374999999999746383, 0.5358532185916217161, 0.4425000000000000044 ) ) ;
#8370 = ORIENTED_EDGE ( 'NONE', *, *, #8853, .F. ) ;
#8371 = CARTESIAN_POINT ( 'NONE',  ( 2.326421213736078119E-17, 0.2258928570453146711, -0.3799334167787516425 ) ) ;
#8372 = CARTESIAN_POINT ( 'NONE',  ( -0.2819296736111111534, 0.08055555547968892838, 0.1167790944451422563 ) ) ;
#8373 = CARTESIAN_POINT ( 'NONE',  ( -0.2764156081756484196, -0.1144950937579609362, -0.06791666666666604235 ) ) ;
#8374 = CARTESIAN_POINT ( 'NONE',  ( -0.3124999999999996114, -0.1294417382415925799, 0.4043055555555600811 ) ) ;
#8375 = CARTESIAN_POINT ( 'NONE',  ( -0.1459302940035950014, -0.2450006702335510156, -0.07419985852680419103 ) ) ;
#8376 = CARTESIAN_POINT ( 'NONE',  ( -0.1144950937579609779, 0.2764156081756484196, 0.3626388888888929518 ) ) ;
#8377 = ORIENTED_EDGE ( 'NONE', *, *, #14555, .T. ) ;
#8378 = CARTESIAN_POINT ( 'NONE',  ( -0.2150490341232084990, 4.620419474169768392, 0.2274236258241670028 ) ) ;
#8379 = DIRECTION ( 'NONE',  ( 0.000000000000000000, 1.000000000000000000, 0.000000000000000000 ) ) ;
#8380 = CC_DESIGN_APPROVAL ( #16403, ( #13854 ) ) ;
#8381 = FACE_OUTER_BOUND ( 'NONE', #10462, .T. ) ;
#8382 = CARTESIAN_POINT ( 'NONE',  ( -0.3119999999999999996, 0.3826388888888884732, 0.1292346314604056190 ) ) ;
#8383 = CARTESIAN_POINT ( 'NONE',  ( -0.2206173157302027676, 5.002166666666665762, 0.2206173157302028787 ) ) ;
#8384 = CARTESIAN_POINT ( 'NONE',  ( 0.1167790944451422702, 4.279944444520309865, -0.2819296736111110979 ) ) ;
#8385 = CARTESIAN_POINT ( 'NONE',  ( 0.2819296736111110979, 4.005638888964754507, -3.452642723725051716E-17 ) ) ;
#8386 = DIRECTION ( 'NONE',  ( 1.000000000000000000, 0.000000000000000000, -0.000000000000000000 ) ) ;
#8387 = CARTESIAN_POINT ( 'NONE',  ( 1.910449006669871087E-17, 0.4208333333333330040, -0.3119999999999999996 ) ) ;
#8388 = CARTESIAN_POINT ( 'NONE',  ( 0.3112018351208193923, 4.807111871885667576, 0.02239305249707624484 ) ) ;
#8389 = ORIENTED_EDGE ( 'NONE', *, *, #16716, .F. ) ;
#8390 = EDGE_LOOP ( 'NONE', ( #11490, #15791, #20808, #9616 ) ) ;
#8391 = CARTESIAN_POINT ( 'NONE',  ( 2.310583317527613811, 2.687712728237018567, -2.461238514389269660 ) ) ;
#8392 = EDGE_CURVE ( 'NONE', #2709, #14964, #22179, .T. ) ;
#8393 = CARTESIAN_POINT ( 'NONE',  ( 0.2819296736111110979, 4.821611111186976828, 0.1167790944451422425 ) ) ;
#8394 = VECTOR ( 'NONE', #2582, 39.37007874015748143 ) ;
#8395 = CARTESIAN_POINT ( 'NONE',  ( -5.488040394358968970E-07, 4.960478275469978549, 0.3119999999989728212 ) ) ;
#8396 = CARTESIAN_POINT ( 'NONE',  ( -0.2393751185404155990, 5.160436163643965735, 0.1810856521565251398 ) ) ;
#8397 = EDGE_CURVE ( 'NONE', #20593, #19663, #5010, .T. ) ;
#8398 = APPROVAL_STATUS ( 'not_yet_approved' ) ;
#8399 = CARTESIAN_POINT ( 'NONE',  ( -0.4687500000000003886, 0.2598076211353315124, 0.06112444011295379426 ) ) ;
#8400 = CARTESIAN_POINT ( 'NONE',  ( 0.1954553509668047195, 0.1954553509668046085, 0.1230555555555576941 ) ) ;
#8401 = CC_DESIGN_SECURITY_CLASSIFICATION ( #4895, ( #24131 ) ) ;
#8402 = CARTESIAN_POINT ( 'NONE',  ( 0.2819296736111111534, 4.168833333409199149, 0.1167790944451422563 ) ) ;
#8403 = PERSON_AND_ORGANIZATION ( #1864, #12741 ) ;
#8404 = CARTESIAN_POINT ( 'NONE',  ( 0.3124999999999999445, -0.1294417382415923856, 0.3070833333333367055 ) ) ;
#8405 = CARTESIAN_POINT ( 'NONE',  ( -0.2764156081756484196, 1.692557448933383907E-17, 0.1508333333333356785 ) ) ;
#8406 = CARTESIAN_POINT ( 'NONE',  ( 0.2233192592356399997, 0.09374999990245758141, -0.3073725909049500049 ) ) ;
#8407 = APPLICATION_CONTEXT ( 'configuration controlled 3d designs of mechanical parts and assemblies' ) ;
#8408 = TOROIDAL_SURFACE ( 'NONE', #22047, 0.2510000000000000009, 0.001000000000000038835 ) ;
#8409 = CARTESIAN_POINT ( 'NONE',  ( -0.2819296736111110979, 0.1222222221463555719, 0.1167790944451422425 ) ) ;
#8410 = CARTESIAN_POINT ( 'NONE',  ( -0.3125000000000000000, 0.1294417382415922468, -0.04708333333333236670 ) ) ;
#8411 = DIRECTION ( 'NONE',  ( -0.000000000000000000, -1.000000000000000000, -0.000000000000000000 ) ) ;
#8412 = CARTESIAN_POINT ( 'NONE',  ( 0.7108475124358174524, 3.066692553488282957, 2.927961747820534644 ) ) ;
#8413 = PLANE ( 'NONE',  #23569 ) ;
#8414 = CARTESIAN_POINT ( 'NONE',  ( 0.2230971623002953874, -0.2230971623002954429, 0.4720138888888936179 ) ) ;
#8415 = CARTESIAN_POINT ( 'NONE',  ( -0.2209708691207961095, 0.2209708691207961373, 0.05361111111111253186 ) ) ;
#8416 = CARTESIAN_POINT ( 'NONE',  ( -0.1571327148983266975, 3.789293766973461430, 0.2726194340734207078 ) ) ;
#8417 = CARTESIAN_POINT ( 'NONE',  ( -0.04084075481946490560, 3.822708396179054446, -0.3120000000000004436 ) ) ;
#8418 = CARTESIAN_POINT ( 'NONE',  ( -0.1167790944451422702, 0.5527777777019111660, -0.2819296736111110424 ) ) ;
#8419 = CARTESIAN_POINT ( 'NONE',  ( -0.1993543840281266355, 4.040361111186976828, 0.1993543840281267465 ) ) ;
#8420 = CARTESIAN_POINT ( 'NONE',  ( -0.1116596296178200276, -0.009821428668970958592, 0.3436530038418508792 ) ) ;
#8421 = ORIENTED_EDGE ( 'NONE', *, *, #24038, .F. ) ;
#8422 = CARTESIAN_POINT ( 'NONE',  ( -0.1993543840281266355, 4.651472222298087544, 0.1993543840281267465 ) ) ;
#8423 = CARTESIAN_POINT ( 'NONE',  ( 0.3999999999999999667, 0.1803571426620580176, -0.1299678784931625197 ) ) ;
#8424 = CARTESIAN_POINT ( 'NONE',  ( 0.3134329418737113460, 4.363010638796406937, 0.009240974733256862236 ) ) ;
#8425 = EDGE_CURVE ( 'NONE', #3858, #16949, #3862, .T. ) ;
#8426 = ORIENTED_EDGE ( 'NONE', *, *, #19915, .F. ) ;
#8427 = ADVANCED_FACE ( 'NONE', ( #3071 ), #2825, .T. ) ;
#8428 = CARTESIAN_POINT ( 'NONE',  ( 2.583392422801337288E-17, 0.1199999999999999956, 0.2109499999999996656 ) ) ;
#8429 = CARTESIAN_POINT ( 'NONE',  ( 5.731347020009612645E-17, 3.849388889040620931, 0.3119999999999999996 ) ) ;
#8430 = CARTESIAN_POINT ( 'NONE',  ( -0.3236067977499789694, -1.707404996040164512E-17, -0.2351141009169893104 ) ) ;
#8431 = VECTOR ( 'NONE', #5954, 39.37007874015748143 ) ;
#8432 = EDGE_CURVE ( 'NONE', #13675, #12402, #1367, .T. ) ;
#8433 = SHAPE_REPRESENTATION_RELATIONSHIP ( 'NONE' , 'NONE' ,  #20236, #23350 ) ;
#8434 = ORIENTED_EDGE ( 'NONE', *, *, #17350, .F. ) ;
#8435 = CARTESIAN_POINT ( 'NONE',  ( 0.1993543840281266633, 4.887583333409199149, -0.1993543840281266910 ) ) ;
#8436 = DATE_TIME_ROLE ( 'classification_date' ) ;
#8437 = ORIENTED_EDGE ( 'NONE', *, *, #6164, .F. ) ;
#8438 = CARTESIAN_POINT ( 'NONE',  ( -0.2777204190475047185, 5.110469173811334365, -0.1386666054842166096 ) ) ;
#8439 = LINE ( 'NONE', #3312, #5408 ) ;
#8440 = EDGE_LOOP ( 'NONE', ( #6856, #11807, #961, #7007 ) ) ;
#8441 = CARTESIAN_POINT ( 'NONE',  ( 0.2819296736111110424, 0.04583333325746670461, 0.1167790944451424923 ) ) ;
#8442 = VERTEX_POINT ( 'NONE', #21599 ) ;
#8443 = CARTESIAN_POINT ( 'NONE',  ( 1.726321361862525858E-17, 0.007638888813022257952, -0.2819296736111110979 ) ) ;
#8444 = DIRECTION ( 'NONE',  ( -0.000000000000000000, -1.000000000000000000, -0.000000000000000000 ) ) ;
#8445 = CARTESIAN_POINT ( 'NONE',  ( 0.02497667677238979075, 4.072372283987069075, 0.3120000032441070936 ) ) ;
#8446 = CARTESIAN_POINT ( 'NONE',  ( -6.979263641208234666E-17, 0.1901785713310290005, 0.3799334167787516425 ) ) ;
#8447 = CARTESIAN_POINT ( 'NONE',  ( -1.910449006669871087E-17, 4.481333333333331836, -0.3119999999999999996 ) ) ;
#8448 = EDGE_CURVE ( 'NONE', #10939, #3183, #18814, .T. ) ;
#8449 = LINE ( 'NONE', #13955, #15851 ) ;
#8450 = VECTOR ( 'NONE', #11684, 39.37007874015748143 ) ;
#8451 = FACE_OUTER_BOUND ( 'NONE', #15091, .T. ) ;
#8452 = CARTESIAN_POINT ( 'NONE',  ( 0.2819296736111110979, 3.825083333409198705, -3.452642723725051716E-17 ) ) ;
#8453 = CARTESIAN_POINT ( 'NONE',  ( 2.356222887430696744, 2.291712385858714729, -2.088288568297006265 ) ) ;
#8454 = CARTESIAN_POINT ( 'NONE',  ( -0.4641327083039736845, -0.2728248698625184154, 0.04698599556840495767 ) ) ;
#8455 = CARTESIAN_POINT ( 'NONE',  ( -0.05195898594955755678, 4.792388845571896816, 0.3076436305813794458 ) ) ;
#8456 = CARTESIAN_POINT ( 'NONE',  ( 0.1292346314604058410, 4.575083333485065573, 0.3119999999999998885 ) ) ;
#8457 = CARTESIAN_POINT ( 'NONE',  ( -0.2819296736111110979, 4.811194444520309865, 0.000000000000000000 ) ) ;
#8458 = ORIENTED_EDGE ( 'NONE', *, *, #19717, .T. ) ;
#8459 = CARTESIAN_POINT ( 'NONE',  ( -0.1993543840281266910, 4.068138888964754507, -0.1993543840281266910 ) ) ;
#8460 = ORIENTED_EDGE ( 'NONE', *, *, #8536, .T. ) ;
#8461 = EDGE_CURVE ( 'NONE', #4893, #6926, #18964, .T. ) ;
#8462 = EDGE_CURVE ( 'NONE', #16532, #12608, #21450, .T. ) ;
#8463 = VERTEX_POINT ( 'NONE', #21839 ) ;
#8464 = VERTEX_POINT ( 'NONE', #5127 ) ;
#8465 = PERSON_AND_ORGANIZATION ( #15518, #2538 ) ;
#8466 = CARTESIAN_POINT ( 'NONE',  ( -0.2209708691207961095, 0.2209708691207961373, 0.06055555555555736796 ) ) ;
#8467 = CARTESIAN_POINT ( 'NONE',  ( 0.1292346314604056745, 0.4729166666666663743, -0.3119999999999999996 ) ) ;
#8468 = EDGE_CURVE ( 'NONE', #7081, #9585, #18542, .T. ) ;
#8469 = CARTESIAN_POINT ( 'NONE',  ( -0.1292346314604056190, 0.02847222207048929338, -0.3119999999999999996 ) ) ;
#8470 = CARTESIAN_POINT ( 'NONE',  ( -0.0004270822970283075638, 4.377178143069785143, -0.3119997496178308904 ) ) ;
#8471 = CARTESIAN_POINT ( 'NONE',  ( -0.4687500000000002220, -0.2630787017013382356, 0.3892820121258429023 ) ) ;
#8472 = CARTESIAN_POINT ( 'NONE',  ( 0.007029742477379865087, 0.1556215347031258134, -0.7499999999999998890 ) ) ;
#8473 = ORIENTED_EDGE ( 'NONE', *, *, #17600, .F. ) ;
#8474 = CARTESIAN_POINT ( 'NONE',  ( 0.2195630361086305937, -0.1679215936616662852, 0.3880822748423153334 ) ) ;
#8475 = CARTESIAN_POINT ( 'NONE',  ( 0.1144950937579611444, 0.2764156081756483641, 0.07097222222222394905 ) ) ;
#8476 = DIRECTION ( 'NONE',  ( -0.000000000000000000, -1.000000000000000000, -0.000000000000000000 ) ) ;
#8477 = CARTESIAN_POINT ( 'NONE',  ( -0.2819296736111110979, 4.352861111186976828, 0.000000000000000000 ) ) ;
#8478 = CARTESIAN_POINT ( 'NONE',  ( -5.731347020009612645E-17, 0.1708333333333330040, 0.3119999999999999996 ) ) ;
#8479 = CARTESIAN_POINT ( 'NONE',  ( -0.1920051058283686329, 0.7214575884338099154, -1.081025299797705008 ) ) ;
#8480 = CARTESIAN_POINT ( 'NONE',  ( 0.000000000000000000, 3.700000000000000622, 0.000000000000000000 ) ) ;
#8481 = CARTESIAN_POINT ( 'NONE',  ( -0.4679361169221507022, 0.2662350510444109197, 0.05893285591566550796 ) ) ;
#8482 = CARTESIAN_POINT ( 'NONE',  ( -0.1292346314604057023, 4.338972222222222008, 0.3119999999999998885 ) ) ;
#8483 = AXIS2_PLACEMENT_3D ( 'NONE', #22238, #11035, #16522 ) ;
#8484 = CARTESIAN_POINT ( 'NONE',  ( 5.731347020009612645E-17, 5.127166666818398610, 0.3119999999999999996 ) ) ;
#8485 = CARTESIAN_POINT ( 'NONE',  ( 0.06745385251108179658, 4.962394104578971898, 0.3046372139198416651 ) ) ;
#8486 = CARTESIAN_POINT ( 'NONE',  ( 0.4593750000000004774, 0.2760455974562900372, 0.06112444011295366936 ) ) ;
#8487 = DIRECTION ( 'NONE',  ( 0.4995222938423188319, 0.04370253788966847047, -0.8651979924482662287 ) ) ;
#8488 = ORIENTED_EDGE ( 'NONE', *, *, #7291, .F. ) ;
#8489 = CARTESIAN_POINT ( 'NONE',  ( -0.5116234456863258950, 1.999640111863030256, -2.727383698113316157 ) ) ;
#8490 = CARTESIAN_POINT ( 'NONE',  ( 0.3013181215143252434, 4.138612934927133225, 0.08484923786493389630 ) ) ;
#8491 = CARTESIAN_POINT ( 'NONE',  ( 0.1306872919485614071, -0.3155070326520293955, -0.02798611111110996946 ) ) ;
#8492 = CARTESIAN_POINT ( 'NONE',  ( -1.726321361862525858E-17, 5.227861111186975940, -0.2819296736111110979 ) ) ;
#8493 = EDGE_CURVE ( 'NONE', #6611, #14624, #10105, .T. ) ;
#8494 = CARTESIAN_POINT ( 'NONE',  ( 0.1571292521837519829, 3.817071648848574306, -0.2726212835620034358 ) ) ;
#8495 =( BOUNDED_CURVE ( )  B_SPLINE_CURVE ( 2, ( #18152, #16323, #3267, #8882, #23735, #21921, #5211, #15461, #20704, #336, #9731, #17171, #20583 ),
 .UNSPECIFIED., .F., .F. ) 
 B_SPLINE_CURVE_WITH_KNOTS ( ( 3, 2, 2, 2, 2, 2, 3 ),
 ( 0.6071428571428572063, 0.6142857142857143238, 0.6285714285714285587, 0.6428571428571429047, 0.6571428571428571397, 0.6714285714285713746, 0.6785714285714286031 ),
 .UNSPECIFIED. ) 
 CURVE ( )  GEOMETRIC_REPRESENTATION_ITEM ( )  RATIONAL_B_SPLINE_CURVE ( ( 0.9755282581475768211, 0.9755282581475769321, 1.000000000000000000, 0.9510565162951535312, 1.000000000000000000, 0.9510565162951535312, 1.000000000000000000, 0.9510565162951535312, 1.000000000000000000, 0.9510565162951535312, 1.000000000000000000, 0.9755282581475765991, 0.9755282581475768211 ) ) 
 REPRESENTATION_ITEM ( '' )  );
#8496 = EDGE_CURVE ( 'NONE', #18946, #13418, #10905, .T. ) ;
#8497 = B_SPLINE_CURVE_WITH_KNOTS ( 'NONE', 3,
 ( #3855, #11299, #191, #7633, #23836, #7157, #9096, #14600, #20203, #5320, #3488, #12784, #1663, #14728, #22143, #12907, #16266, #16391, #21626, #1267, #8584, #20040, #8693, #14560, #16143, #1508, #3328, #5278, #19673, #14316, #7241, #6748, #10902, #12502, #12258, #5034, #19799, #23558, #12383, #16021, #8943, #10786, #2974, #1145, #8817, #3210, #18213, #6997 ),
 .UNSPECIFIED., .F., .F.,
 ( 4, 2, 2, 2, 2, 2, 2, 2, 2, 2, 2, 2, 2, 2, 2, 2, 2, 2, 2, 2, 2, 2, 2, 4 ),
 ( 0.002493122863401542495, 0.004000377874406220446, 0.004754005379908560723, 0.005507632885410900132, 0.007014887896415579818, 0.007768515401917921830, 0.008522142907420263841, 0.009275770412922604985, 0.01002939791842494613, 0.01153665292942963189, 0.01229028043493197303, 0.01304390794043431417, 0.01455116295143899993, 0.01530479045694134108, 0.01605841796244368222, 0.01756567297344836798, 0.01907292798445305027, 0.01982655548995539141, 0.02058018299545773255, 0.02208743800646241831, 0.02359469301746710060, 0.02510194802847178636, 0.02585557553397412750, 0.02660920303947646864 ),
 .UNSPECIFIED. ) ;
#8498 = CARTESIAN_POINT ( 'NONE',  ( 0.1116596296178199027, 0.1223214284738861762, 0.3436530038418508792 ) ) ;
#8499 = CARTESIAN_POINT ( 'NONE',  ( -0.2819296736111110979, 0.1291666665908000611, -0.1167790944451423396 ) ) ;
#8500 = CARTESIAN_POINT ( 'NONE',  ( 0.000000000000000000, 0.2764156081756484196, -0.02972222222222129645 ) ) ;
#8501 = FACE_OUTER_BOUND ( 'NONE', #12916, .T. ) ;
#8502 = CARTESIAN_POINT ( 'NONE',  ( 2.725416254512337932, 0.04999999999999973910, -2.591000000000000636 ) ) ;
#8503 = CARTESIAN_POINT ( 'NONE',  ( -0.1144950937579609918, -0.2764156081756484196, 0.3279166666666703533 ) ) ;
#8504 = ORIENTED_EDGE ( 'NONE', *, *, #16212, .F. ) ;
#8505 = DIRECTION ( 'NONE',  ( 1.224646799147353207E-16, 1.000000000000000000, -0.000000000000000000 ) ) ;
#8506 = DIRECTION ( 'NONE',  ( -0.5773502691896278405, 0.5773502691896214012, 0.5773502691896278405 ) ) ;
#8507 = CARTESIAN_POINT ( 'NONE',  ( 0.000000000000000000, 5.384999999999999787, 0.000000000000000000 ) ) ;
#8508 = CARTESIAN_POINT ( 'NONE',  ( 0.2206173157302027676, 0.3999999999999996336, 0.2206173157302028787 ) ) ;
#8509 = CARTESIAN_POINT ( 'NONE',  ( -0.1292346314604056745, 4.984805555555555934, -0.3119999999999999996 ) ) ;
#8510 = CC_DESIGN_DATE_AND_TIME_ASSIGNMENT ( #6855, #16607, ( #11937 ) ) ;
#8511 = CARTESIAN_POINT ( 'NONE',  ( -0.1993543840281266355, 4.248694444520309865, 0.1993543840281267465 ) ) ;
#8512 = CARTESIAN_POINT ( 'NONE',  ( 0.1167790944451424368, 3.939666666742532186, 0.2819296736111110424 ) ) ;
#8513 = PLANE ( 'NONE',  #22101 ) ;
#8514 = CARTESIAN_POINT ( 'NONE',  ( -0.3119999999999998885, 3.887583333333332725, 0.1292346314604058410 ) ) ;
#8515 = CARTESIAN_POINT ( 'NONE',  ( 0.3568845019303670818, 1.003480569432281344E-17, 0.06134667963492219933 ) ) ;
#8516 = EDGE_LOOP ( 'NONE', ( #14323, #3081, #1520, #2059 ) ) ;
#8517 = ORIENTED_EDGE ( 'NONE', *, *, #21130, .T. ) ;
#8518 = AXIS2_PLACEMENT_3D ( 'NONE', #11123, #3433, #10886 ) ;
#8519 = CARTESIAN_POINT ( 'NONE',  ( -0.2726213461307027686, 3.997589792078371396, -0.1571291336435313157 ) ) ;
#8520 = CARTESIAN_POINT ( 'NONE',  ( -0.1167790944451423257, 4.564666666742531298, -0.2819296736111110424 ) ) ;
#8521 = CARTESIAN_POINT ( 'NONE',  ( -0.1116596296178199582, 0.01517857133102903239, -0.3436530038418508792 ) ) ;
#8522 = CARTESIAN_POINT ( 'NONE',  ( -0.1068925302184129816, 4.491398126007289271, -0.2939241610522889125 ) ) ;
#8523 = PERSON_AND_ORGANIZATION ( #15518, #2538 ) ;
#8524 = LINE ( 'NONE', #3044, #7640 ) ;
#8525 = CARTESIAN_POINT ( 'NONE',  ( 0.1954553509668046640, -0.1954553509668047195, -0.05749999999999928085 ) ) ;
#8526 = CARTESIAN_POINT ( 'NONE',  ( 0.1993543840281267465, 3.998694444520310753, 0.1993543840281266633 ) ) ;
#8527 = DATE_AND_TIME ( #17444, #12332 ) ;
#8528 = CARTESIAN_POINT ( 'NONE',  ( -0.04965346344051063676, 4.823057060546735997, -0.3081848164328563899 ) ) ;
#8529 = CYLINDRICAL_SURFACE ( 'NONE', #12534, 0.4000000000000000222 ) ;
#8530 = CARTESIAN_POINT ( 'NONE',  ( -0.1954553509668046918, -0.1954553509668046640, 0.1022222222222241989 ) ) ;
#8531 = CARTESIAN_POINT ( 'NONE',  ( 0.2233192592356399997, 0.1651785713310289783, -0.3073725909049500049 ) ) ;
#8532 = VECTOR ( 'NONE', #5274, 39.37007874015748143 ) ;
#8533 = CARTESIAN_POINT ( 'NONE',  ( 0.1993543840281266910, 0.04236111103524448085, -0.1993543840281266910 ) ) ;
#8534 = CARTESIAN_POINT ( 'NONE',  ( 0.4800180224839157850, -0.1716599939501584626, 0.06108543995043075325 ) ) ;
#8535 = CARTESIAN_POINT ( 'NONE',  ( 0.4795759075923620163, -5.969813580926603513E-13, 0.07439896364136204532 ) ) ;
#8536 = EDGE_CURVE ( 'NONE', #9670, #12181, #18661, .T. ) ;
#8537 = DIRECTION ( 'NONE',  ( 0.4985709748471340297, 0.07555085810113193467, -0.8635502596144368770 ) ) ;
#8538 = CARTESIAN_POINT ( 'NONE',  ( 0.2472135954999579721, 0.3392857142857140795, -0.3402603233408159622 ) ) ;
#8539 = CARTESIAN_POINT ( 'NONE',  ( -3.863846776457871776E-17, -0.3155070326520292845, 0.2984027777777810697 ) ) ;
#8540 = VERTEX_POINT ( 'NONE', #10755 ) ;
#8541 = LINE ( 'NONE', #15983, #1324 ) ;
#8542 = CARTESIAN_POINT ( 'NONE',  ( -0.05083916931420053020, 3.767441789872082669, -0.3079993799698920731 ) ) ;
#8543 = FACE_OUTER_BOUND ( 'NONE', #1675, .T. ) ;
#8544 = CARTESIAN_POINT ( 'NONE',  ( 1.726321361862525858E-17, 0.4381944443685778512, -0.2819296736111110979 ) ) ;
#8545 = CARTESIAN_POINT ( 'NONE',  ( 0.1993543840281267465, 4.109805555631421470, 0.1993543840281266633 ) ) ;
#8546 = CARTESIAN_POINT ( 'NONE',  ( 0.3613381517857143232, -0.05625000009754237834, -0.1174058825155740587 ) ) ;
#8547 = EDGE_LOOP ( 'NONE', ( #13676, #22357, #9069, #3904 ) ) ;
#8548 = EDGE_CURVE ( 'NONE', #4825, #5409, #6346, .T. ) ;
#8549 = CARTESIAN_POINT ( 'NONE',  ( -0.2819296736111110424, 4.648000000075866112, 0.1167790944451424923 ) ) ;
#8550 = PRODUCT_DEFINITION_SHAPE ( 'NONE', 'NONE',  #10901 ) ;
#8551 = FACE_OUTER_BOUND ( 'NONE', #3555, .T. ) ;
#8552 = CARTESIAN_POINT ( 'NONE',  ( 0.1746784157998219900, 5.086973785772764600, -0.2585344347967651335 ) ) ;
#8553 = ORIENTED_EDGE ( 'NONE', *, *, #16516, .F. ) ;
#8554 = DIRECTION ( 'NONE',  ( -0.4999999999999911737, 2.705315378517703502E-18, 0.8660254037844437036 ) ) ;
#8555 = CARTESIAN_POINT ( 'NONE',  ( -1.726321361862525858E-17, 5.116750000075865223, -0.2819296736111110979 ) ) ;
#8556 = CARTESIAN_POINT ( 'NONE',  ( 0.03651601414450977162, -0.2739930093161348501, 0.3880822748423153890 ) ) ;
#8557 = AXIS2_PLACEMENT_3D ( 'NONE', #11628, #16984, #276 ) ;
#8558 =( NAMED_UNIT ( * ) PLANE_ANGLE_UNIT ( ) SI_UNIT ( $, .RADIAN. ) );
#8559 = ORIENTED_EDGE ( 'NONE', *, *, #9740, .F. ) ;
#8560 = CARTESIAN_POINT ( 'NONE',  ( 1.726321361862525858E-17, 0.6048611110352445364, -0.2819296736111110979 ) ) ;
#8561 = CARTESIAN_POINT ( 'NONE',  ( 0.1993543840281266633, 4.832027777853643791, -0.1993543840281266910 ) ) ;
#8562 = CALENDAR_DATE ( 2026, 7, 10 ) ;
#8563 = CARTESIAN_POINT ( 'NONE',  ( 1.910449006669871087E-17, 0.3027777776260448528, -0.3119999999999999996 ) ) ;
#8564 = EDGE_CURVE ( 'NONE', #14213, #17904, #16232, .T. ) ;
#8565 = CARTESIAN_POINT ( 'NONE',  ( -0.07317740563318354818, 4.569553305210725114, 0.3034604867065505696 ) ) ;
#8566 = VERTEX_POINT ( 'NONE', #22561 ) ;
#8567 = CARTESIAN_POINT ( 'NONE',  ( 0.2819296736111110424, 0.3861111110352444808, -0.1167790944451423119 ) ) ;
#8568 = EDGE_CURVE ( 'NONE', #20678, #10349, #5714, .T. ) ;
#8569 = ADVANCED_FACE ( 'NONE', ( #7918 ), #11841, .T. ) ;
#8570 = FACE_OUTER_BOUND ( 'NONE', #17703, .T. ) ;
#8571 = CARTESIAN_POINT ( 'NONE',  ( -0.1292346314604056190, 0.3131944444444441089, -0.3119999999999999996 ) ) ;
#8572 = CARTESIAN_POINT ( 'NONE',  ( -0.5116234456863466562, 3.685658299244018998, 2.728348793029228059 ) ) ;
#8573 = CARTESIAN_POINT ( 'NONE',  ( 2.326421213736078119E-17, 0.2973214284738861513, -0.3799334167787516425 ) ) ;
#8574 = CARTESIAN_POINT ( 'NONE',  ( -0.2817863736917600725, 5.053780319418576639, -0.1342011136461285226 ) ) ;
#8575 = VECTOR ( 'NONE', #9852, 39.37007874015748143 ) ;
#8576 = DIRECTION ( 'NONE',  ( 0.8660254037844432595, 0.000000000000000000, -0.4999999999999916733 ) ) ;
#8577 = VECTOR ( 'NONE', #18247, 39.37007874015748854 ) ;
#8578 = CARTESIAN_POINT ( 'NONE',  ( -0.1167790944451423257, 4.800777777853643791, -0.2819296736111110424 ) ) ;
#8579 = VERTEX_POINT ( 'NONE', #22797 ) ;
#8580 = CARTESIAN_POINT ( 'NONE',  ( 1.644486777265590005, 2.661358883302036293, -2.047525463909579457 ) ) ;
#8581 = ORIENTED_EDGE ( 'NONE', *, *, #1721, .F. ) ;
#8582 = EDGE_CURVE ( 'NONE', #5165, #2652, #13198, .T. ) ;
#8583 = CARTESIAN_POINT ( 'NONE',  ( 5.178964085587577574E-17, 3.866750000075865668, 0.2819296736111110979 ) ) ;
#8584 = CARTESIAN_POINT ( 'NONE',  ( -0.2851672621379254258, 0.05388838813870399508, 0.1040316926689665855 ) ) ;
#8585 = CARTESIAN_POINT ( 'NONE',  ( 0.03417214391962999920, 5.016978872011788937, 0.3101611866967836084 ) ) ;
#8586 = CARTESIAN_POINT ( 'NONE',  ( -0.4692112248683376619, -0.2611554184491534092, 0.04763613967037600566 ) ) ;
#8587 = CARTESIAN_POINT ( 'NONE',  ( 0.8119709581221709049, 2.291712385858714729, -1.528283969076322801 ) ) ;
#8588 = CARTESIAN_POINT ( 'NONE',  ( -0.3119999999999998885, 4.227861111262844140, 0.1292346314604058410 ) ) ;
#8589 = CARTESIAN_POINT ( 'NONE',  ( -0.2819296736111110424, 4.814666666742533074, 0.1167790944451424923 ) ) ;
#8590 = ORIENTED_EDGE ( 'NONE', *, *, #11416, .F. ) ;
#8591 = CARTESIAN_POINT ( 'NONE',  ( -0.2819296736111110979, 4.019527777853642903, 0.000000000000000000 ) ) ;
#8592 = VERTEX_POINT ( 'NONE', #19259 ) ;
#8593 = ORIENTED_EDGE ( 'NONE', *, *, #19915, .T. ) ;
#8595 = EDGE_CURVE ( 'NONE', #22303, #18060, #19095, .T. ) ;
#8594 = VECTOR ( 'NONE', #15779, 39.37007874015748143 ) ;
#8596 = VECTOR ( 'NONE', #5955, 39.37007874015748854 ) ;
#8597 = ORIENTED_EDGE ( 'NONE', *, *, #10667, .F. ) ;
#8598 = APPROVAL_STATUS ( 'not_yet_approved' ) ;
#8599 = CARTESIAN_POINT ( 'NONE',  ( -0.1294417382415922191, 0.3125000000000000000, 0.05708333333333515114 ) ) ;
#8600 = CARTESIAN_POINT ( 'NONE',  ( 1.457716030923678074, 2.291712385858714729, -2.174029041877829194 ) ) ;
#8601 = ORIENTED_EDGE ( 'NONE', *, *, #1259, .T. ) ;
#8602 = CARTESIAN_POINT ( 'NONE',  ( 0.2206173157302028232, 0.3513888887371559577, -0.2206173157302028232 ) ) ;
#8603 = FACE_OUTER_BOUND ( 'NONE', #23174, .T. ) ;
#8604 = CARTESIAN_POINT ( 'NONE',  ( 0.06924143819089124963, 0.5799707351147035395, -0.7469066312677832276 ) ) ;
#8605 = ORIENTED_EDGE ( 'NONE', *, *, #9881, .F. ) ;
#8606 = CARTESIAN_POINT ( 'NONE',  ( 4.113055369932088708E-16, 0.1589285712334866096, 0.4000000000000000222 ) ) ;
#8607 = CARTESIAN_POINT ( 'NONE',  ( 0.2819296736111110979, 0.09444444436857780956, -0.1167790944451422980 ) ) ;
#8608 = CARTESIAN_POINT ( 'NONE',  ( -0.1144950937579609918, -0.2764156081756484196, 0.1543055555555579716 ) ) ;
#8609 = CARTESIAN_POINT ( 'NONE',  ( 0.1167790944451424368, 4.425777777853643791, 0.2819296736111110424 ) ) ;
#8610 = CARTESIAN_POINT ( 'NONE',  ( -0.3125000000000000000, -0.1294417382415921913, 0.3973611111111152727 ) ) ;
#8611 = CARTESIAN_POINT ( 'NONE',  ( -0.1395219119112078299, 0.2093243512325797528, -1.227272371974961418 ) ) ;
#8612 = CARTESIAN_POINT ( 'NONE',  ( 0.2209708691207961095, -0.2209708691207961651, -0.02972222222222147686 ) ) ;
#8613 = CARTESIAN_POINT ( 'NONE',  ( -0.4687500000000004441, 0.2629256801278679334, 0.05975678175779900597 ) ) ;
#8614 = CARTESIAN_POINT ( 'NONE',  ( 0.2206173157302028787, 4.016055555555555046, 0.2206173157302027954 ) ) ;
#8615 = TOROIDAL_SURFACE ( 'NONE', #12135, 1.015181661097394050, 0.03500000000000000333 ) ;
#8616 = CARTESIAN_POINT ( 'NONE',  ( -0.1292346314604057023, 5.123694444596177178, 0.3119999999999998885 ) ) ;
#8617 = CARTESIAN_POINT ( 'NONE',  ( 0.2101503697800941040, 4.967001120964043004, 0.2322385514659185413 ) ) ;
#8618 = ORIENTED_EDGE ( 'NONE', *, *, #20351, .F. ) ;
#8619 = ORIENTED_EDGE ( 'NONE', *, *, #18218, .F. ) ;
#8620 = CARTESIAN_POINT ( 'NONE',  ( -0.3125000000000004996, 0.1294417382415917195, 0.2306944444444476439 ) ) ;
#8621 = CARTESIAN_POINT ( 'NONE',  ( -0.1306872919485614903, 0.3155070326520293400, 0.1109027777777800150 ) ) ;
#8622 = CARTESIAN_POINT ( 'NONE',  ( 0.000000000000000000, 5.384999999999999787, 0.000000000000000000 ) ) ;
#8623 = CARTESIAN_POINT ( 'NONE',  ( 0.3038794415728064968, 3.805497571066078777, 0.08166545862924670662 ) ) ;
#8624 = CARTESIAN_POINT ( 'NONE',  ( -0.3613381517857144343, 0.1758928570453146822, 0.1174058825155740171 ) ) ;
#8625 = CARTESIAN_POINT ( 'NONE',  ( 0.2819296736111110424, 0.1013888888130222571, 0.1167790944451424923 ) ) ;
#8626 = CARTESIAN_POINT ( 'NONE',  ( -3.385114897866767815E-17, -0.2764156081756484196, 0.05361111111111271227 ) ) ;
#8627 = LINE ( 'NONE', #9995, #674 ) ;
#8628 = CARTESIAN_POINT ( 'NONE',  ( -0.1993543840281266355, 5.151472222298088433, 0.1993543840281267465 ) ) ;
#8629 = CARTESIAN_POINT ( 'NONE',  ( -3.385114897866767815E-17, -0.2764156081756484196, 0.3869444444444486431 ) ) ;
#8630 = ADVANCED_FACE ( 'NONE', ( #9887 ), #10011, .T. ) ;
#8631 = CARTESIAN_POINT ( 'NONE',  ( 0.000000000000000000, 5.384999999999999787, 0.000000000000000000 ) ) ;
#8632 = CARTESIAN_POINT ( 'NONE',  ( 0.2472135954999579166, 0.1035714285714285227, 0.3402603233408160732 ) ) ;
#8633 = LINE ( 'NONE', #16078, #18398 ) ;
#8634 = CARTESIAN_POINT ( 'NONE',  ( -0.2206173157302028787, 0.4972222222222218435, 0.2206173157302027954 ) ) ;
#8635 = CARTESIAN_POINT ( 'NONE',  ( -0.3119999999999998885, 4.720916666666666650, 0.1292346314604058410 ) ) ;
#8636 = CARTESIAN_POINT ( 'NONE',  ( 0.1993543840281267465, 4.207027777853643791, 0.1993543840281266633 ) ) ;
#8637 = CARTESIAN_POINT ( 'NONE',  ( 0.1167790944451424368, 3.995222222298087988, 0.2819296736111110424 ) ) ;
#8638 = CARTESIAN_POINT ( 'NONE',  ( 0.000000000000000000, 0.05000000000000028727, -0.5991858428704237571 ) ) ;
#8639 = CARTESIAN_POINT ( 'NONE',  ( -0.4254812175018319320, 0.2956141819054338149, 0.4012599972956991667 ) ) ;
#8640 = CARTESIAN_POINT ( 'NONE',  ( 7.484242640931070629E-07, 4.016084960865516251, 0.3119999999981048489 ) ) ;
#8641 = CARTESIAN_POINT ( 'NONE',  ( -0.1993543840281266910, 4.457027777853642903, -0.1993543840281266910 ) ) ;
#8642 = CARTESIAN_POINT ( 'NONE',  ( -0.2401696643338466775, 4.508321440767591781, 0.1991626441011656312 ) ) ;
#8643 = SECURITY_CLASSIFICATION_LEVEL ( 'unclassified' ) ;
#8644 = CARTESIAN_POINT ( 'NONE',  ( -0.4645343760433822689, -0.2721270390806222461, 0.05893285591566541776 ) ) ;
#8645 = CARTESIAN_POINT ( 'NONE',  ( -0.1954553509668046918, -0.1954553509668046640, 0.09527777777777970969 ) ) ;
#8646 = CARTESIAN_POINT ( 'NONE',  ( 0.1167790944451424506, 4.106333333409199149, 0.2819296736111110424 ) ) ;
#8647 = CARTESIAN_POINT ( 'NONE',  ( -0.01743693570811869625, 4.822118045354796045, -0.3115821376521073494 ) ) ;
#8648 = CARTESIAN_POINT ( 'NONE',  ( -3.385114897866767815E-17, -0.2764156081756484196, 0.2758333333333366499 ) ) ;
#8649 = CARTESIAN_POINT ( 'NONE',  ( 0.2923287055106771337, 0.004464285616743311064, 0.2123892367102621359 ) ) ;
#8650 = CARTESIAN_POINT ( 'NONE',  ( -0.1993543840281266633, 0.05624999992413336897, -0.1993543840281266910 ) ) ;
#8651 = LINE ( 'NONE', #19757, #15613 ) ;
#8652 = CARTESIAN_POINT ( 'NONE',  ( -0.4795759075923621273, -5.504308098328212156E-13, 0.07439896364136201756 ) ) ;
#8653 = DIRECTION ( 'NONE',  ( 0.000000000000000000, 0.000000000000000000, -1.000000000000000000 ) ) ;
#8654 = CARTESIAN_POINT ( 'NONE',  ( -0.1954553509668046640, 0.1954553509668046918, 0.08138888888889070361 ) ) ;
#8655 = CARTESIAN_POINT ( 'NONE',  ( -3.863846776457871776E-17, -0.3155070326520292845, 0.3539583333333371495 ) ) ;
#8656 = ORIENTED_EDGE ( 'NONE', *, *, #6661, .F. ) ;
#8657 = ORIENTED_EDGE ( 'NONE', *, *, #1812, .F. ) ;
#8658 = CARTESIAN_POINT ( 'NONE',  ( -0.5116234456863466562, 3.514980167629567998, 2.722575290337332365 ) ) ;
#8659 = CARTESIAN_POINT ( 'NONE',  ( 1.059513921322799533E-10, 3.821611107313654720, -0.3119999999999999996 ) ) ;
#8660 = CARTESIAN_POINT ( 'NONE',  ( 1.726321361862525858E-17, 0.4937499999241333759, -0.2819296736111110979 ) ) ;
#8661 = CARTESIAN_POINT ( 'NONE',  ( -0.1993543840281266910, 3.970916666742532186, -0.1993543840281266910 ) ) ;
#8662 = CARTESIAN_POINT ( 'NONE',  ( 0.3613381517857143232, -0.05982142866897095096, 0.000000000000000000 ) ) ;
#8663 = AXIS2_PLACEMENT_3D ( 'NONE', #23022, #6323, #10121 ) ;
#8664 = CARTESIAN_POINT ( 'NONE',  ( -1.726321361862525858E-17, 4.575083333409199149, -0.2819296736111110979 ) ) ;
#8665 = DIRECTION ( 'NONE',  ( 0.000000000000000000, 0.000000000000000000, 1.000000000000000000 ) ) ;
#8666 = CARTESIAN_POINT ( 'NONE',  ( 0.3121506383504715210, 5.078286358898017383, 0.009141518313334958193 ) ) ;
#8667 = PLANE ( 'NONE',  #6607 ) ;
#8668 = CARTESIAN_POINT ( 'NONE',  ( 0.1292346314604058410, 3.741750000151732536, 0.3119999999999998885 ) ) ;
#8669 = CARTESIAN_POINT ( 'NONE',  ( 0.2677787189661461897, 4.191816329952293252, 0.1601340282671347148 ) ) ;
#8670 = EDGE_CURVE ( 'NONE', #10191, #4025, #6896, .T. ) ;
#8671 = ORIENTED_EDGE ( 'NONE', *, *, #3467, .F. ) ;
#8672 = CARTESIAN_POINT ( 'NONE',  ( 0.03458881943681251653, 5.206640035683668621, 0.2803355776336168281 ) ) ;
#8673 = CARTESIAN_POINT ( 'NONE',  ( 0.1167790944451424506, 4.981333333409198261, 0.2819296736111110424 ) ) ;
#8674 = PERSON_AND_ORGANIZATION ( #15518, #2538 ) ;
#8675 = ORIENTED_EDGE ( 'NONE', *, *, #342, .F. ) ;
#8676 = AXIS2_PLACEMENT_3D ( 'NONE', #12148, #21750, #23079 ) ;
#8677 = EDGE_CURVE ( 'NONE', #16468, #2585, #17255, .T. ) ;
#8678 = CARTESIAN_POINT ( 'NONE',  ( -0.2933685965344436375, 5.111756720891555084, -0.1009642549206684198 ) ) ;
#8679 = CARTESIAN_POINT ( 'NONE',  ( -0.008838905694748024067, 4.571396606871324764, 0.3119999992378313380 ) ) ;
#8680 = ORIENTED_EDGE ( 'NONE', *, *, #11798, .F. ) ;
#8681 = CARTESIAN_POINT ( 'NONE',  ( -0.2819296736111110979, 0.1881944443685777957, -3.452642723725051716E-17 ) ) ;
#8682 = VERTEX_POINT ( 'NONE', #15959 ) ;
#8683 = CARTESIAN_POINT ( 'NONE',  ( -0.2819296736111110979, 0.08055555547968892838, 0.1167790944451422425 ) ) ;
#8684 = DIRECTION ( 'NONE',  ( -0.000000000000000000, -1.000000000000000000, -0.000000000000000000 ) ) ;
#8685 = CARTESIAN_POINT ( 'NONE',  ( -0.2826589919575409060, 5.202197775706403071, 0.03072956325641070657 ) ) ;
#8686 = CARTESIAN_POINT ( 'NONE',  ( -0.3999999999999999667, -0.06785714285714286587, -0.1299678784931626030 ) ) ;
#8687 = CARTESIAN_POINT ( 'NONE',  ( -0.2015210671123849329, 5.065410029797029701, 0.2392828963600910630 ) ) ;
#8688 = CARTESIAN_POINT ( 'NONE',  ( -0.4795759075923621273, -5.504308098328212156E-13, 0.07439896364136201756 ) ) ;
#8689 = DIRECTION ( 'NONE',  ( 0.000000000000000000, 0.000000000000000000, -1.000000000000000000 ) ) ;
#8690 = CARTESIAN_POINT ( 'NONE',  ( 0.2819296736111110979, 4.783416666742532186, -3.452642723725051716E-17 ) ) ;
#8691 = CARTESIAN_POINT ( 'NONE',  ( 1.519200945994765378E-06, 3.766055514889470324, -0.3119999999963013471 ) ) ;
#8692 = CARTESIAN_POINT ( 'NONE',  ( 0.1015009281151166981, 3.724843158531562892, -0.2819296736111110979 ) ) ;
#8693 = CARTESIAN_POINT ( 'NONE',  ( -0.2934558719060931797, 0.05332506518006699392, 0.07539210639951753057 ) ) ;
#8694 = CARTESIAN_POINT ( 'NONE',  ( -5.731347020009612645E-17, 0.1083333331816004053, 0.3119999999999999996 ) ) ;
#8695 = CARTESIAN_POINT ( 'NONE',  ( -0.4570242136016807732, -0.2774028246161672762, 0.04874733047933989954 ) ) ;
#8696 = CARTESIAN_POINT ( 'NONE',  ( 3.073863465859856523E-17, 0.4997679491924311157, -0.2510000000000000009 ) ) ;
#8697 = CARTESIAN_POINT ( 'NONE',  ( 0.2206173157302027954, 4.370222222373953969, -0.2206173157302028232 ) ) ;
#8698 = VECTOR ( 'NONE', #20610, 39.37007874015748143 ) ;
#8699 = CARTESIAN_POINT ( 'NONE',  ( -0.2819296736111110979, 4.696611111186977716, -0.1167790944451422980 ) ) ;
#8700 = VERTEX_POINT ( 'NONE', #4858 ) ;
#8701 = EDGE_CURVE ( 'NONE', #17157, #15989, #21146, .T. ) ;
#8702 = CARTESIAN_POINT ( 'NONE',  ( -0.1993543840281266355, 3.804250000075865223, 0.1993543840281267465 ) ) ;
#8703 = EDGE_CURVE ( 'NONE', #5136, #3473, #23030, .T. ) ;
#8704 = PERSON_AND_ORGANIZATION_ROLE ( 'creator' ) ;
#8705 = ADVANCED_FACE ( 'NONE', ( #4973 ), #4623, .T. ) ;
#8706 = DIRECTION ( 'NONE',  ( -0.000000000000000000, -1.000000000000000000, -0.000000000000000000 ) ) ;
#8707 = CARTESIAN_POINT ( 'NONE',  ( 0.2209708691207961095, -0.2209708691207961651, 0.2550000000000033906 ) ) ;
#8708 = ORIENTED_EDGE ( 'NONE', *, *, #8254, .T. ) ;
#8709 = CARTESIAN_POINT ( 'NONE',  ( -5.731347020009612645E-17, 0.3861111109593781676, 0.3119999999999999996 ) ) ;
#8710 = B_SPLINE_CURVE_WITH_KNOTS ( 'NONE', 1,
 ( #9650, #17086 ),
 .UNSPECIFIED., .F., .F.,
 ( 2, 2 ),
 ( 0.000000000000000000, 1.000000000000000000 ),
 .UNSPECIFIED. ) ;
#8711 = CARTESIAN_POINT ( 'NONE',  ( 0.3060819870398079900, 1.999640111863030478, -2.785681210928895535 ) ) ;
#8712 = AXIS2_PLACEMENT_3D ( 'NONE', #9054, #10535, #14679 ) ;
#8713 = CARTESIAN_POINT ( 'NONE',  ( -0.4687500000000003886, -0.1103614930154983020, 0.4107126734332217644 ) ) ;
#8714 = CARTESIAN_POINT ( 'NONE',  ( -0.06335377612981497875, 0.3482590814838159021, -0.3999999999999999667 ) ) ;
#8715 = EDGE_LOOP ( 'NONE', ( #15524, #15842, #11032, #18341 ) ) ;
#8716 = DIRECTION ( 'NONE',  ( -0.000000000000000000, 1.000000000000000000, -0.000000000000000000 ) ) ;
#8717 = CARTESIAN_POINT ( 'NONE',  ( -0.2819296736111110979, 0.2854166665908000611, -3.452642723725051716E-17 ) ) ;
#8718 = CARTESIAN_POINT ( 'NONE',  ( 0.2764156081756484196, -5.077672346800151106E-17, 0.005000000000001210074 ) ) ;
#8719 = CARTESIAN_POINT ( 'NONE',  ( 5.178964085587577574E-17, 4.533416666742532186, 0.2819296736111110979 ) ) ;
#8720 = CARTESIAN_POINT ( 'NONE',  ( 0.2872991414527151233, 0.07488537861673724705, -0.08546435887091462236 ) ) ;
#8721 = DIRECTION ( 'NONE',  ( 0.000000000000000000, 1.000000000000000000, 0.000000000000000000 ) ) ;
#8722 = CARTESIAN_POINT ( 'NONE',  ( -1.960390272410463459E-06, 4.210500054279665783, -0.3119999999938410928 ) ) ;
#8723 = CARTESIAN_POINT ( 'NONE',  ( 0.1292346314604058410, 4.068138888888888083, 0.3119999999999998885 ) ) ;
#8724 = CARTESIAN_POINT ( 'NONE',  ( 0.2206173157302027954, 4.870222222373954857, -0.2206173157302028232 ) ) ;
#8725 = EDGE_CURVE ( 'NONE', #24096, #22560, #23382, .T. ) ;
#8726 = EDGE_CURVE ( 'NONE', #19405, #22848, #6331, .T. ) ;
#8727 = EDGE_LOOP ( 'NONE', ( #4084, #15016, #19028, #18073 ) ) ;
#8728 = LINE ( 'NONE', #7275, #4675 ) ;
#8729 = CARTESIAN_POINT ( 'NONE',  ( 1.201146141948970407E-06, 4.904991752689871198, 0.3119999999951060254 ) ) ;
#8730 =( BOUNDED_CURVE ( )  B_SPLINE_CURVE ( 2, ( #12789, #11064, #16307, #1551, #8987, #1788, #16550, #22028, #7043, #16432, #23842, #7162, #5325 ),
 .UNSPECIFIED., .F., .F. ) 
 B_SPLINE_CURVE_WITH_KNOTS ( ( 3, 2, 2, 2, 2, 2, 3 ),
 ( 0.2500000000000000000, 0.2571428571428571175, 0.2714285714285714080, 0.2857142857142856984, 0.2999999999999999889, 0.3142857142857142794, 0.3214285714285714524 ),
 .UNSPECIFIED. ) 
 CURVE ( )  GEOMETRIC_REPRESENTATION_ITEM ( )  RATIONAL_B_SPLINE_CURVE ( ( 0.9755282581475768211, 0.9755282581475768211, 1.000000000000000000, 0.9510565162951535312, 1.000000000000000000, 0.9510565162951535312, 1.000000000000000000, 0.9510565162951535312, 1.000000000000000000, 0.9510565162951535312, 1.000000000000000000, 0.9755282581475765991, 0.9755282581475767101 ) ) 
 REPRESENTATION_ITEM ( '' )  );
#8731 = EDGE_CURVE ( 'NONE', #19257, #23449, #19498, .T. ) ;
#8732 = CARTESIAN_POINT ( 'NONE',  ( -0.3155070326520292845, 1.931923388228935888E-17, 0.2324305555555587766 ) ) ;
#8733 = CARTESIAN_POINT ( 'NONE',  ( 0.000000000000000000, 0.000000000000000000, 0.7500000000000001110 ) ) ;
#8734 = ORIENTED_EDGE ( 'NONE', *, *, #21743, .F. ) ;
#8735 = CARTESIAN_POINT ( 'NONE',  ( -0.1292346314604081170, 4.429249999999999687, -0.3119999999999975016 ) ) ;
#8736 = CARTESIAN_POINT ( 'NONE',  ( 0.3613381517857143232, 0.2116071427596004084, -0.1174058825155740587 ) ) ;
#8737 = CARTESIAN_POINT ( 'NONE',  ( 0.1167790944451423535, 0.1499999999241333759, 0.2819296736111110979 ) ) ;
#8738 = CARTESIAN_POINT ( 'NONE',  ( 0.1144950937579611444, 0.2764156081756483641, 0.02236111111111246247 ) ) ;
#8739 = CARTESIAN_POINT ( 'NONE',  ( 0.2819296736111110424, 5.175777777853644679, -0.1167790944451423396 ) ) ;
#8740 = CARTESIAN_POINT ( 'NONE',  ( -0.1144950937579609918, -0.2764156081756484196, 0.4390277777777824020 ) ) ;
#8741 = AXIS2_PLACEMENT_3D ( 'NONE', #15816, #8131, #4356 ) ;
#8742 = ORIENTED_EDGE ( 'NONE', *, *, #16450, .F. ) ;
#8743 = CARTESIAN_POINT ( 'NONE',  ( -0.1908862062913858626, 4.605243227715043908, -0.2467925334992447373 ) ) ;
#8744 = CARTESIAN_POINT ( 'NONE',  ( -0.1178635634473103738, 4.269440902833853357, -0.2905642712132933125 ) ) ;
#8745 = CARTESIAN_POINT ( 'NONE',  ( 1.573500000000000343, -3.414809992080329023E-17, -0.3524999999999999800 ) ) ;
#8746 = CARTESIAN_POINT ( 'NONE',  ( -0.3119999999999999996, 0.5493055555555551583, 0.1292346314604056190 ) ) ;
#8747 = CARTESIAN_POINT ( 'NONE',  ( 0.1292346314604056190, 4.811194444444443441, -0.3119999999999999996 ) ) ;
#8748 = CARTESIAN_POINT ( 'NONE',  ( 0.1340080504559709729, 5.203643142954044620, 0.2502513067613080788 ) ) ;
#8749 = CARTESIAN_POINT ( 'NONE',  ( -0.2819296736111110979, 4.019527777853642903, 0.000000000000000000 ) ) ;
#8750 = CARTESIAN_POINT ( 'NONE',  ( -0.1166234456863465552, 3.066692553488282957, 2.711183489075826181 ) ) ;
#8751 = PLANE ( 'NONE',  #9254 ) ;
#8752 = CARTESIAN_POINT ( 'NONE',  ( 0.3119999999999998885, 0.5076388887371560132, 0.1292346314604058410 ) ) ;
#8753 = LOCAL_TIME ( 21, 9, 13.00000000000000000, #10376 ) ;
#8754 = ORIENTED_EDGE ( 'NONE', *, *, #1780, .T. ) ;
#8755 = CARTESIAN_POINT ( 'NONE',  ( 0.1292346314604031765, 3.922305555555555490, -0.3120000000000024420 ) ) ;
#8756 = CARTESIAN_POINT ( 'NONE',  ( 0.2819296736111110979, 4.547305555631421470, -3.452642723725051716E-17 ) ) ;
#8757 = CARTESIAN_POINT ( 'NONE',  ( -0.3089083532858699077, 4.500952954266654871, -0.04389791046443763944 ) ) ;
#8758 = B_SPLINE_CURVE_WITH_KNOTS ( 'NONE', 3,
 ( #454, #14980, #17283, #20579, #15458, #22765, #22650, #3876 ),
 .UNSPECIFIED., .F., .F.,
 ( 4, 2, 2, 4 ),
 ( 1.149246120147598830E-16, 0.002297969625094406759, 0.003446954437641552675, 0.004595939250188698158 ),
 .UNSPECIFIED. ) ;
#8759 = EDGE_CURVE ( 'NONE', #18060, #3460, #23930, .T. ) ;
#8760 = AXIS2_PLACEMENT_3D ( 'NONE', #12065, #14967, #16793 ) ;
#8761 = EDGE_CURVE ( 'NONE', #15581, #23410, #18667, .T. ) ;
#8762 = COORDINATED_UNIVERSAL_TIME_OFFSET ( 0, 0, .AHEAD. ) ;
#8763 = CARTESIAN_POINT ( 'NONE',  ( -0.1229229017546027425, -0.2477443904639724803, -0.06558227484231506088 ) ) ;
#8764 = CARTESIAN_POINT ( 'NONE',  ( -0.1144950937579609779, 0.2764156081756484196, 0.02236111111111246247 ) ) ;
#8765 = CARTESIAN_POINT ( 'NONE',  ( -0.2819296736111110424, 4.148000000075866112, 0.1167790944451424923 ) ) ;
#8766 = CARTESIAN_POINT ( 'NONE',  ( -0.3125000000000000000, 1.913510623667739771E-17, -0.05055555555555497210 ) ) ;
#8767 = CARTESIAN_POINT ( 'NONE',  ( -0.3119999999999998885, 4.887583333333332725, 0.1292346314604058410 ) ) ;
#8768 = CARTESIAN_POINT ( 'NONE',  ( 0.2764156081756483641, 0.1144950937579610195, 0.2931944444444479214 ) ) ;
#8769 = LOCAL_TIME ( 21, 9, 13.00000000000000000, #6520 ) ;
#8770 = CARTESIAN_POINT ( 'NONE',  ( 0.1116596296178199860, 0.09732142847388616791, -0.3436530038418508792 ) ) ;
#8771 = CARTESIAN_POINT ( 'NONE',  ( 0.2819296736111110424, 0.08749999992413336203, 0.1167790944451424923 ) ) ;
#8772 = LINE ( 'NONE', #12341, #12513 ) ;
#8773 = DIRECTION ( 'NONE',  ( 0.000000000000000000, 0.000000000000000000, 1.000000000000000000 ) ) ;
#8774 = PLANE ( 'NONE',  #1577 ) ;
#8775 = CARTESIAN_POINT ( 'NONE',  ( 0.000000000000000000, 0.2764156081756484196, 0.01888888888889020401 ) ) ;
#8776 = CARTESIAN_POINT ( 'NONE',  ( 0.3155070326520292290, 0.1306872919485615736, 0.3713194444444484765 ) ) ;
#8777 = ORIENTED_EDGE ( 'NONE', *, *, #5573, .T. ) ;
#8778 = ORIENTED_EDGE ( 'NONE', *, *, #13957, .T. ) ;
#8779 = CARTESIAN_POINT ( 'NONE',  ( 0.3885631146789285117, 0.3299392016703767139, 0.06110928887248361085 ) ) ;
#8780 = MANIFOLD_SOLID_BREP ( '1/2-13 Machine Threads Stud2', #15051 ) ;
#8781 = CARTESIAN_POINT ( 'NONE',  ( 1.573500000000000343, 0.05625000000000004996, -1.818749999999999867 ) ) ;
#8782 = CARTESIAN_POINT ( 'NONE',  ( -0.2819296736111110979, 0.5111111110352446474, 0.1167790944451422425 ) ) ;
#8783 = CARTESIAN_POINT ( 'NONE',  ( -0.1993543840281266910, 3.915361111186976384, -0.1993543840281266910 ) ) ;
#8784 = CARTESIAN_POINT ( 'NONE',  ( 0.2233192592356399164, 0.07232142847388618734, 0.3073725909049500604 ) ) ;
#8785 = ORIENTED_EDGE ( 'NONE', *, *, #10668, .T. ) ;
#8786 = CARTESIAN_POINT ( 'NONE',  ( 0.2819296736111110424, 4.342444444520311642, -0.1167790944451423396 ) ) ;
#8787 = CARTESIAN_POINT ( 'NONE',  ( 0.01997118933809540267, 5.142873989094642440, -0.3040754418437698892 ) ) ;
#8788 = CARTESIAN_POINT ( 'NONE',  ( -0.3119999999999999996, 0.1465277776260448528, -0.1292346314604056745 ) ) ;
#8789 = ORIENTED_EDGE ( 'NONE', *, *, #10680, .T. ) ;
#8790 = CARTESIAN_POINT ( 'NONE',  ( -0.1993543840281266355, 5.137583333409198261, 0.1993543840281267465 ) ) ;
#8791 = PRODUCT_DEFINITION ( 'UNKNOWN', '', #11526, #21188 ) ;
#8792 = CC_DESIGN_APPROVAL ( #20442, ( #2926 ) ) ;
#8793 = CARTESIAN_POINT ( 'NONE',  ( -0.5116234456863466562, 3.514980167629567998, 2.549370209580444246 ) ) ;
#8794 = AXIS2_PLACEMENT_3D ( 'NONE', #5218, #21696, #3274 ) ;
#8795 = CARTESIAN_POINT ( 'NONE',  ( -0.2819296736111110979, 4.849388888964755395, -0.1167790944451422980 ) ) ;
#8796 = PERSON_AND_ORGANIZATION_ROLE ( 'classification_officer' ) ;
#8797 = VERTEX_POINT ( 'NONE', #10369 ) ;
#8798 = AXIS2_PLACEMENT_3D ( 'NONE', #17251, #7972, #16884 ) ;
#8799 = SPHERICAL_SURFACE ( 'NONE', #19501, 0.7650000000000000133 ) ;
#8800 = CARTESIAN_POINT ( 'NONE',  ( -0.1876229909954430231, 4.549487878473160052, -0.2524456540483745459 ) ) ;
#8801 = ORIENTED_EDGE ( 'NONE', *, *, #4382, .T. ) ;
#8802 = EDGE_CURVE ( 'NONE', #17046, #22531, #12869, .T. ) ;
#8803 = CARTESIAN_POINT ( 'NONE',  ( 0.1993543840281266910, 0.2784722221463555858, -0.1993543840281266910 ) ) ;
#8804 = EDGE_LOOP ( 'NONE', ( #4667, #2394, #8906, #10199, #2248 ) ) ;
#8805 = CARTESIAN_POINT ( 'NONE',  ( 0.2819296736111110424, 0.04583333325746670461, 0.1167790944451424923 ) ) ;
#8806 = LINE ( 'NONE', #16012, #5709 ) ;
#8807 = CARTESIAN_POINT ( 'NONE',  ( -0.3866234456863466007, 2.661589509557314326, 2.621538993229147962 ) ) ;
#8808 = CARTESIAN_POINT ( 'NONE',  ( 0.3236067977499790249, 0.04999999999999996114, -0.2351141009169892826 ) ) ;
#8809 = CARTESIAN_POINT ( 'NONE',  ( -0.2434908057415208216, 5.063736957178592846, 0.1953540873034801117 ) ) ;
#8810 = LINE ( 'NONE', #23671, #12643 ) ;
#8811 = CARTESIAN_POINT ( 'NONE',  ( -0.3115168255710737966, 3.890354268893235989, -0.02373096174760461544 ) ) ;
#8812 = APPROVAL_PERSON_ORGANIZATION ( #16725, #23253, #13205 ) ;
#8813 = LINE ( 'NONE', #4674, #19364 ) ;
#8814 = CARTESIAN_POINT ( 'NONE',  ( 0.1167790944451424368, 4.495222222298088433, 0.2819296736111110424 ) ) ;
#8815 = CARTESIAN_POINT ( 'NONE',  ( 0.001849798306578129140, 4.543780820092050199, -0.3119953020238740438 ) ) ;
#8816 = CARTESIAN_POINT ( 'NONE',  ( -0.1993543840281266910, 3.790361111186976828, -0.1993543840281266910 ) ) ;
#8817 = CARTESIAN_POINT ( 'NONE',  ( -0.03933790649247456001, 0.04385992660403156135, -0.2908781100274356324 ) ) ;
#8818 = CARTESIAN_POINT ( 'NONE',  ( 0.3096594984987066645, 3.751112016665212767, 0.03836432376948438472 ) ) ;
#8819 = DIRECTION ( 'NONE',  ( 0.000000000000000000, -5.763336813132313106E-16, -1.000000000000000000 ) ) ;
#8820 = ORIENTED_EDGE ( 'NONE', *, *, #21838, .T. ) ;
#8821 = AXIS2_PLACEMENT_3D ( 'NONE', #16575, #14630, #4982 ) ;
#8822 = CARTESIAN_POINT ( 'NONE',  ( -0.07317541673116574608, 4.791775583817363682, 0.3034609665091877462 ) ) ;
#8823 = CC_DESIGN_PERSON_AND_ORGANIZATION_ASSIGNMENT ( #17267, #13734, ( #7598 ) ) ;
#8824 = CARTESIAN_POINT ( 'NONE',  ( -0.3119999999999999996, 4.391055555707287894, 0.000000000000000000 ) ) ;
#8825 = CARTESIAN_POINT ( 'NONE',  ( -0.2819296736111110979, 4.644527777853643791, 0.000000000000000000 ) ) ;
#8826 = CARTESIAN_POINT ( 'NONE',  ( -0.2819296736111110424, 3.904944444520309865, -0.1167790944451423119 ) ) ;
#8827 = VERTEX_POINT ( 'NONE', #21691 ) ;
#8828 = CALENDAR_DATE ( 2026, 7, 10 ) ;
#8829 = CARTESIAN_POINT ( 'NONE',  ( 0.03750733961385147031, -0.5077191469176455252, 0.4064695056028757025 ) ) ;
#8830 = CARTESIAN_POINT ( 'NONE',  ( -3.827021247335479543E-17, -0.3125000000000000000, 0.2480555555555588598 ) ) ;
#8831 = ORIENTED_EDGE ( 'NONE', *, *, #23305, .F. ) ;
#8832 = CARTESIAN_POINT ( 'NONE',  ( 0.2206173157302027676, 0.1708333331816004053, 0.2206173157302028787 ) ) ;
#8833 = CIRCLE ( 'NONE', #3388, 0.09499999999999995948 ) ;
#8834 = CARTESIAN_POINT ( 'NONE',  ( -0.0008552964370042808167, 4.377189652761055427, -0.3119989957290913996 ) ) ;
#8835 = CARTESIAN_POINT ( 'NONE',  ( -0.1964023011945066899, 3.716541689590819431, -0.2424612127253647220 ) ) ;
#8836 = PLANE ( 'NONE',  #5288 ) ;
#8837 = CARTESIAN_POINT ( 'NONE',  ( -0.1236067977499789583, 0.3499999999999998668, -0.3804226065180614791 ) ) ;
#8838 =( BOUNDED_CURVE ( )  B_SPLINE_CURVE ( 2, ( #1342, #8410, #15858, #6830, #1225, #10616, #21707, #1464, #18046 ),
 .UNSPECIFIED., .F., .T. ) 
 B_SPLINE_CURVE_WITH_KNOTS ( ( 3, 2, 2, 2, 3 ),
 ( 0.7395833333333333703, 0.7500000000000000000, 0.7604166666666667407, 0.7708333333333334814, 0.7812500000000001110 ),
 .UNSPECIFIED. ) 
 CURVE ( )  GEOMETRIC_REPRESENTATION_ITEM ( )  RATIONAL_B_SPLINE_CURVE ( ( 1.000000000000000000, 0.9238795325112867385, 1.000000000000000000, 0.9238795325112867385, 1.000000000000000000, 0.9238795325112867385, 1.000000000000000000, 0.9238795325112859613, 1.000000000000000888 ) ) 
 REPRESENTATION_ITEM ( '' )  );
#8839 = ORIENTED_EDGE ( 'NONE', *, *, #967, .T. ) ;
#8840 =( BOUNDED_SURFACE ( )  B_SPLINE_SURFACE ( 1, 2, ( 
 ( #20274, #24037, #9053, #3927, #10893, #3808, #7232, #16499, #11254, #2094, #18560, #23791, #16734, #3685, #22458, #5757, #16618, #7463, #11132, #13218, #23911, #20628, #7111, #11372, #13100, #12737, #1850, #3442, #7347, #14799, #5634, #14677, #22214, #22096, #5392, #3561, #14912, #20513, #5514, #9293, #18799, #9536, #21975, #12976, #15, #18678, #1979, #9417, #16854, #141, #264, #23046, #22933, #6107, #20749, #7704, #2464, #11862, #4163, #9658, #19277, #5868, #18929, #22696, #20986, #11613, #19045, #20869, #9903, #6229, #7935, #2347, #383, #17334, #628, #6352, #11987, #15389, #4041, #15151, #11494, #22817, #17452, #2583, #13802, #9785, #15507, #2227, #13576, #22580, #17217, #13327, #21111, #501, #8059, #2698, #4282, #11737, #10030, #17097, #19158, #13693, #4400, #16969, #7823, #746, #8174, #15269, #15628, #19400, #21233, #4524, #5987, #13451, #23402, #21470, #8295, #17574, #19635, #4754, #8539, #15980, #4878, #19761, #15862, #21583, #23518, #12225, #17935, #16104, #4995, #21711, #2811, #23277, #2934, #1346, #8655, #12345, #5113, #10266, #12580, #8776, #3171, #1105, #864, #6957, #4642, #10392, #21823, #12459, #13924, #3056, #1229, #985, #6710, #10503, #6834, #14154, #14275, #19877, #10621, #18050, #15749, #17814, #20001, #16229, #23640, #14399, #10150, #23160, #8414, #6470, #6591, #21352, #12108, #19518, #17692, #14040, #22065 ),
 ( #12825, #14643, #1703, #9141, #22184, #12949, #9025, #14768, #16704, #5359, #11098, #9264, #22302, #14884, #20122, #16465, #20244, #18650, #1819, #5484, #22426, #3413, #5728, #1942, #20482, #18410, #18172, #111, #21941, #3533, #15004, #5599, #7080, #20360, #18529, #18292, #16586, #3651, #24123, #7318, #7437, #13064, #3778, #24007, #1468, #10984, #13187, #11221, #9389, #16829, #7552, #3288, #1589, #10742, #23877, #14519, #8903, #16347, #23759, #5234, #12707, #10863, #7198, #9750, #238, #11341, #6079, #15477, #7795, #13304, #22903, #9506, #22550, #2197, #473, #15239, #22668, #354, #13545, #2432, #11588, #5956, #4015, #20960, #4253, #9997, #15595, #19017, #7674, #18770, #15124, #2313, #21078, #6197, #17422, #13416, #19128, #5841, #17187, #2066, #20839, #16940, #594, #4131, #11705, #6319, #7904, #15356, #13663, #20719, #22785, #9874, #17301, #20600, #11463, #8026, #4368, #18896, #11825, #23017, #2549, #9628, #19245, #17061, #715, #8143, #3897, #15713, #21438, #2667, #19485, #8263, #4843, #12309, #17659, #8503, #4963, #19842, #18018, #19369, #16196, #6678, #14123, #946, #1071, #8376, #23610, #17779, #4723, #1316, #4610, #2895, #8629, #10117, #12430, #14243, #12195, #17903, #10232, #19723, #23246, #17542, #19602, #15943, #21552, #3026, #3141, #8740, #12072, #15827, #10473, #6555, #2779, #10591, #10355, #1197, #835, #14005, #16074 ) ),
 .UNSPECIFIED., .F., .F., .F. ) 
 B_SPLINE_SURFACE_WITH_KNOTS ( ( 2, 2 ),
 ( 3, 2, 2, 2, 2, 2, 2, 2, 2, 2, 2, 2, 2, 2, 2, 2, 2, 2, 2, 2, 2, 2, 2, 2, 2, 2, 2, 2, 2, 2, 2, 2, 2, 2, 2, 2, 2, 2, 2, 2, 2, 2, 2, 2, 2, 2, 2, 2, 2, 2, 2, 2, 2, 2, 2, 2, 2, 2, 2, 2, 2, 2, 2, 2, 2, 2, 2, 2, 2, 2, 2, 2, 2, 2, 2, 2, 2, 2, 2, 2, 2, 2, 2, 2, 2, 2, 2, 2, 2, 3 ),
 ( 0.000000000000000000, 1.000000000000000000 ),
 ( 0.000000000000000000, 0.01041666666666666609, 0.02083333333333333218, 0.03125000000000000000, 0.04166666666666666435, 0.05208333333333333565, 0.06250000000000000000, 0.07291666666666667129, 0.08333333333333332871, 0.09375000000000000000, 0.1041666666666666713, 0.1145833333333333287, 0.1250000000000000000, 0.1354166666666666574, 0.1458333333333333426, 0.1562500000000000000, 0.1666666666666666574, 0.1770833333333333426, 0.1875000000000000000, 0.1979166666666666574, 0.2083333333333333426, 0.2187500000000000000, 0.2291666666666666574, 0.2395833333333333426, 0.2500000000000000000, 0.2604166666666666852, 0.2708333333333333148, 0.2812500000000000000, 0.2916666666666666852, 0.3020833333333333148, 0.3125000000000000000, 0.3229166666666666852, 0.3333333333333333148, 0.3437500000000000000, 0.3541666666666666852, 0.3645833333333333148, 0.3750000000000000000, 0.3854166666666666852, 0.3958333333333333148, 0.4062500000000000000, 0.4166666666666666852, 0.4270833333333333148, 0.4375000000000000000, 0.4479166666666666852, 0.4583333333333333148, 0.4687500000000000000, 0.4791666666666666852, 0.4895833333333333148, 0.5000000000000000000, 0.5104166666666666297, 0.5208333333333333703, 0.5312500000000000000, 0.5416666666666666297, 0.5520833333333333703, 0.5625000000000000000, 0.5729166666666666297, 0.5833333333333333703, 0.5937500000000000000, 0.6041666666666666297, 0.6145833333333333703, 0.6250000000000000000, 0.6354166666666666297, 0.6458333333333333703, 0.6562500000000000000, 0.6666666666666666297, 0.6770833333333333703, 0.6875000000000000000, 0.6979166666666666297, 0.7083333333333333703, 0.7187500000000000000, 0.7291666666666666297, 0.7395833333333333703, 0.7500000000000000000, 0.7604166666666666297, 0.7708333333333333703, 0.7812500000000000000, 0.7916666666666666297, 0.8020833333333333703, 0.8125000000000000000, 0.8229166666666666297, 0.8333333333333333703, 0.8437500000000000000, 0.8541666666666666297, 0.8645833333333333703, 0.8750000000000000000, 0.8854166666666666297, 0.8958333333333333703, 0.9062500000000000000, 0.9166666666666666297, 0.9270833333333333703 ),
 .UNSPECIFIED. ) 
 GEOMETRIC_REPRESENTATION_ITEM ( )  RATIONAL_B_SPLINE_SURFACE ( (
 ( 1.000000000000000000, 0.9238795325112867385, 1.000000000000000000, 0.9238795325112867385, 1.000000000000000000, 0.9238795325112867385, 1.000000000000000000, 0.9238795325112867385, 1.000000000000000000, 0.9238795325112867385, 1.000000000000000000, 0.9238795325112867385, 1.000000000000000000, 0.9238795325112867385, 1.000000000000000000, 0.9238795325112867385, 1.000000000000000000, 0.9238795325112867385, 1.000000000000000000, 0.9238795325112867385, 1.000000000000000000, 0.9238795325112867385, 1.000000000000000000, 0.9238795325112867385, 1.000000000000000000, 0.9238795325112867385, 1.000000000000000000, 0.9238795325112867385, 1.000000000000000000, 0.9238795325112867385, 1.000000000000000000, 0.9238795325112867385, 1.000000000000000000, 0.9238795325112867385, 1.000000000000000000, 0.9238795325112867385, 1.000000000000000000, 0.9238795325112867385, 1.000000000000000000, 0.9238795325112867385, 1.000000000000000000, 0.9238795325112867385, 1.000000000000000000, 0.9238795325112867385, 1.000000000000000000, 0.9238795325112867385, 1.000000000000000000, 0.9238795325112867385, 1.000000000000000000, 0.9238795325112867385, 1.000000000000000000, 0.9238795325112867385, 1.000000000000000000, 0.9238795325112867385, 1.000000000000000000, 0.9238795325112867385, 1.000000000000000000, 0.9238795325112867385, 1.000000000000000000, 0.9238795325112867385, 1.000000000000000000, 0.9238795325112867385, 1.000000000000000000, 0.9238795325112867385, 1.000000000000000000, 0.9238795325112867385, 1.000000000000000000, 0.9238795325112867385, 1.000000000000000000, 0.9238795325112867385, 1.000000000000000000, 0.9238795325112867385, 1.000000000000000000, 0.9238795325112867385, 1.000000000000000000, 0.9238795325112867385, 1.000000000000000000, 0.9238795325112867385, 1.000000000000000000, 0.9238795325112867385, 1.000000000000000000, 0.9238795325112867385, 1.000000000000000000, 0.9238795325112867385, 1.000000000000000000, 0.9238795325112867385, 1.000000000000000000, 0.9238795325112867385, 1.000000000000000000, 0.9238795325112867385, 1.000000000000000000, 0.9238795325112867385, 1.000000000000000000, 0.9238795325112867385, 1.000000000000000000, 0.9238795325112867385, 1.000000000000000000, 0.9238795325112867385, 1.000000000000000000, 0.9238795325112867385, 1.000000000000000000, 0.9238795325112867385, 1.000000000000000000, 0.9238795325112867385, 1.000000000000000000, 0.9238795325112867385, 1.000000000000000000, 0.9238795325112867385, 1.000000000000000000, 0.9238795325112867385, 1.000000000000000000, 0.9238795325112867385, 1.000000000000000000, 0.9238795325112867385, 1.000000000000000000, 0.9238795325112867385, 1.000000000000000000, 0.9238795325112867385, 1.000000000000000000, 0.9238795325112867385, 1.000000000000000000, 0.9238795325112867385, 1.000000000000000000, 0.9238795325112867385, 1.000000000000000000, 0.9238795325112867385, 1.000000000000000000, 0.9238795325112867385, 1.000000000000000000, 0.9238795325112867385, 1.000000000000000000, 0.9238795325112867385, 1.000000000000000000, 0.9238795325112867385, 1.000000000000000000, 0.9238795325112867385, 1.000000000000000000, 0.9238795325112867385, 1.000000000000000000, 0.9238795325112867385, 1.000000000000000000, 0.9238795325112867385, 1.000000000000000000, 0.9238795325112867385, 1.000000000000000000, 0.9238795325112867385, 1.000000000000000000, 0.9238795325112867385, 1.000000000000000000, 0.9238795325112867385, 1.000000000000000000, 0.9238795325112867385, 1.000000000000000000, 0.9238795325112867385, 1.000000000000000000, 0.9238795325112867385, 1.000000000000000000, 0.9238795325112867385, 1.000000000000000000, 0.9238795325112867385, 1.000000000000000000, 0.9238795325112867385, 1.000000000000000000, 0.9238795325112867385, 1.000000000000000000, 0.9238795325112867385, 1.000000000000000000, 0.9238795325112867385, 1.000000000000000000, 0.9238795325112867385, 1.000000000000000000, 0.9238795325112867385, 1.000000000000000000, 0.9238795325112867385, 1.000000000000000000, 0.9238795325112867385, 1.000000000000000000, 0.9238795325112867385, 1.000000000000000000),
 ( 1.000000000000000000, 0.9238795325112867385, 1.000000000000000000, 0.9238795325112867385, 1.000000000000000000, 0.9238795325112867385, 1.000000000000000000, 0.9238795325112867385, 1.000000000000000000, 0.9238795325112867385, 1.000000000000000000, 0.9238795325112867385, 1.000000000000000000, 0.9238795325112867385, 1.000000000000000000, 0.9238795325112867385, 1.000000000000000000, 0.9238795325112867385, 1.000000000000000000, 0.9238795325112867385, 1.000000000000000000, 0.9238795325112867385, 1.000000000000000000, 0.9238795325112867385, 1.000000000000000000, 0.9238795325112867385, 1.000000000000000000, 0.9238795325112867385, 1.000000000000000000, 0.9238795325112867385, 1.000000000000000000, 0.9238795325112867385, 1.000000000000000000, 0.9238795325112867385, 1.000000000000000000, 0.9238795325112867385, 1.000000000000000000, 0.9238795325112867385, 1.000000000000000000, 0.9238795325112867385, 1.000000000000000000, 0.9238795325112867385, 1.000000000000000000, 0.9238795325112867385, 1.000000000000000000, 0.9238795325112867385, 1.000000000000000000, 0.9238795325112867385, 1.000000000000000000, 0.9238795325112867385, 1.000000000000000000, 0.9238795325112867385, 1.000000000000000000, 0.9238795325112867385, 1.000000000000000000, 0.9238795325112867385, 1.000000000000000000, 0.9238795325112867385, 1.000000000000000000, 0.9238795325112867385, 1.000000000000000000, 0.9238795325112867385, 1.000000000000000000, 0.9238795325112867385, 1.000000000000000000, 0.9238795325112867385, 1.000000000000000000, 0.9238795325112867385, 1.000000000000000000, 0.9238795325112867385, 1.000000000000000000, 0.9238795325112867385, 1.000000000000000000, 0.9238795325112867385, 1.000000000000000000, 0.9238795325112867385, 1.000000000000000000, 0.9238795325112867385, 1.000000000000000000, 0.9238795325112867385, 1.000000000000000000, 0.9238795325112867385, 1.000000000000000000, 0.9238795325112867385, 1.000000000000000000, 0.9238795325112867385, 1.000000000000000000, 0.9238795325112867385, 1.000000000000000000, 0.9238795325112867385, 1.000000000000000000, 0.9238795325112867385, 1.000000000000000000, 0.9238795325112867385, 1.000000000000000000, 0.9238795325112867385, 1.000000000000000000, 0.9238795325112867385, 1.000000000000000000, 0.9238795325112867385, 1.000000000000000000, 0.9238795325112867385, 1.000000000000000000, 0.9238795325112867385, 1.000000000000000000, 0.9238795325112867385, 1.000000000000000000, 0.9238795325112867385, 1.000000000000000000, 0.9238795325112867385, 1.000000000000000000, 0.9238795325112867385, 1.000000000000000000, 0.9238795325112867385, 1.000000000000000000, 0.9238795325112867385, 1.000000000000000000, 0.9238795325112867385, 1.000000000000000000, 0.9238795325112867385, 1.000000000000000000, 0.9238795325112867385, 1.000000000000000000, 0.9238795325112867385, 1.000000000000000000, 0.9238795325112867385, 1.000000000000000000, 0.9238795325112867385, 1.000000000000000000, 0.9238795325112867385, 1.000000000000000000, 0.9238795325112867385, 1.000000000000000000, 0.9238795325112867385, 1.000000000000000000, 0.9238795325112867385, 1.000000000000000000, 0.9238795325112867385, 1.000000000000000000, 0.9238795325112867385, 1.000000000000000000, 0.9238795325112867385, 1.000000000000000000, 0.9238795325112867385, 1.000000000000000000, 0.9238795325112867385, 1.000000000000000000, 0.9238795325112867385, 1.000000000000000000, 0.9238795325112867385, 1.000000000000000000, 0.9238795325112867385, 1.000000000000000000, 0.9238795325112867385, 1.000000000000000000, 0.9238795325112867385, 1.000000000000000000, 0.9238795325112867385, 1.000000000000000000, 0.9238795325112867385, 1.000000000000000000, 0.9238795325112867385, 1.000000000000000000, 0.9238795325112867385, 1.000000000000000000, 0.9238795325112867385, 1.000000000000000000, 0.9238795325112867385, 1.000000000000000000, 0.9238795325112867385, 1.000000000000000000, 0.9238795325112867385, 1.000000000000000000, 0.9238795325112867385, 1.000000000000000000, 0.9238795325112867385, 1.000000000000000000, 0.9238795325112867385, 1.000000000000000000) ) ) 
 REPRESENTATION_ITEM ( '' )  SURFACE ( )  );
#8841 = CARTESIAN_POINT ( 'NONE',  ( 0.2206057284202265489, 5.078575579926999595, 0.2213988795958710953 ) ) ;
#8842 = CARTESIAN_POINT ( 'NONE',  ( 0.2819296736111110979, 0.2055555554796889006, -0.1167790944451422980 ) ) ;
#8843 = CARTESIAN_POINT ( 'NONE',  ( -3.385114897866767815E-17, -0.2764156081756484196, 0.2688888888888921747 ) ) ;
#8844 = ORIENTED_EDGE ( 'NONE', *, *, #17678, .F. ) ;
#8845 = ADVANCED_FACE ( 'NONE', ( #1329 ), #21923, .T. ) ;
#8846 = CARTESIAN_POINT ( 'NONE',  ( -0.1167790944451423535, 4.474388888964753619, 0.2819296736111110424 ) ) ;
#8847 = CARTESIAN_POINT ( 'NONE',  ( 0.1292346314604056745, 0.1951388888888886119, -0.3119999999999999996 ) ) ;
#8848 = FACE_OUTER_BOUND ( 'NONE', #5008, .T. ) ;
#8849 = CARTESIAN_POINT ( 'NONE',  ( -0.1706684928076038221, 4.233164261868517464, 0.2620792061749219748 ) ) ;
#8850 = CARTESIAN_POINT ( 'NONE',  ( -0.3119999999999998885, 4.109805555555554157, 0.1292346314604058410 ) ) ;
#8851 = DIRECTION ( 'NONE',  ( 0.000000000000000000, 1.000000000000000000, 0.000000000000000000 ) ) ;
#8852 = CARTESIAN_POINT ( 'NONE',  ( 0.2206173157302027954, 5.036888889040620931, -0.2206173157302028232 ) ) ;
#8853 = EDGE_CURVE ( 'NONE', #15906, #960, #23331, .T. ) ;
#8854 = VECTOR ( 'NONE', #8576, 39.37007874015748143 ) ;
#8855 = CARTESIAN_POINT ( 'NONE',  ( -0.1292346314604057300, 4.172305555555555046, 0.3119999999999998885 ) ) ;
#8856 = ORIENTED_EDGE ( 'NONE', *, *, #18218, .T. ) ;
#8857 = CARTESIAN_POINT ( 'NONE',  ( -0.2062328096137425182, 4.883584785677744122, -0.2343418988765107736 ) ) ;
#8858 = CARTESIAN_POINT ( 'NONE',  ( 0.3155070326520292290, -0.1306872919485616569, 0.2567361111111144956 ) ) ;
#8859 = CARTESIAN_POINT ( 'NONE',  ( 0.2923287055106771337, 0.4330357141881717720, 0.2123892367102621359 ) ) ;
#8860 = B_SPLINE_CURVE_WITH_KNOTS ( 'NONE', 3,
 ( #5700, #13163, #14614, #22038, #18265, #20577, #16441, #7053, #3874, #11317, #14490, #21913, #5205, #12678, #12799, #3384, #1561, #11565, #15456, #20937, #7770, #18993, #17281, #22879, #4345, #21056, #2172, #22648, #20817, #693, #8004, #4230, #4465, #9605, #11929, #8119, #2528, #452, #212, #6298, #3988, #7651, #4106, #5936, #9726, #13394, #17164, #11439, #13751, #20698, #13638, #17036, #330, #11799, #19348, #11682 ),
 .UNSPECIFIED., .F., .F.,
 ( 4, 2, 1, 1, 1, 1, 1, 1, 2, 2, 2, 2, 2, 2, 2, 2, 1, 2, 2, 2, 2, 2, 2, 2, 1, 2, 2, 2, 2, 2, 2, 4 ),
 ( 0.2284379164993652067, 0.2284424888044066237, 0.2284470611094480408, 0.2284562057195309026, 0.2284744949396965985, 0.2285110733800279903, 0.2285842302606907739, 0.2287305440220163133, 0.2290231715446674476, 0.2296084265899696608, 0.2307789366805741149, 0.2319494467711785690, 0.2331199568617830231, 0.2342904669523874772, 0.2348757219976896904, 0.2351683495203407970, 0.2353146632816663641, 0.2353878201623291477, 0.2354243986026605395, 0.2354609770429919313, 0.2378019972242008118, 0.2401430174054097200, 0.2413135274960141741, 0.2418987825413164150, 0.2421914100639675216, 0.2423377238252930610, 0.2424108807059558446, 0.2424840375866186282, 0.2436545476772231378, 0.2448250577678276474, 0.2459955678584321292, 0.2471660779490366389 ),
 .UNSPECIFIED. ) ;
#8861 = ORIENTED_EDGE ( 'NONE', *, *, #6632, .F. ) ;
#8862 = CARTESIAN_POINT ( 'NONE',  ( 0.8208141571295791694, 2.690000000000002167, -2.986000000000000210 ) ) ;
#8863 = EDGE_CURVE ( 'NONE', #3289, #22427, #581, .T. ) ;
#8864 = CARTESIAN_POINT ( 'NONE',  ( -0.1116596296178199582, 0.2294642856167432854, -0.3436530038418508792 ) ) ;
#8865 = ADVANCED_FACE ( 'NONE', ( #10845 ), #5094, .T. ) ;
#8866 = EDGE_CURVE ( 'NONE', #17266, #20417, #1805, .T. ) ;
#8867 = AXIS2_PLACEMENT_3D ( 'NONE', #14530, #5245, #18302 ) ;
#8868 = CARTESIAN_POINT ( 'NONE',  ( -0.2819296736111111534, 0.3583333332574666907, 0.1167790944451422563 ) ) ;
#8869 = CARTESIAN_POINT ( 'NONE',  ( 0.2764156081756483641, 0.1144950937579610056, 0.2376388888888919526 ) ) ;
#8870 = CARTESIAN_POINT ( 'NONE',  ( -0.2819296736111110424, 5.092444444520309865, 0.1167790944451424923 ) ) ;
#8871 = CARTESIAN_POINT ( 'NONE',  ( 0.1818344428640181754, 4.482884648730991906, -0.2543617637045067492 ) ) ;
#8872 = EDGE_LOOP ( 'NONE', ( #38, #4420, #12364, #15192 ) ) ;
#8873 = CARTESIAN_POINT ( 'NONE',  ( 0.000000000000000000, 5.384999999999999787, 0.000000000000000000 ) ) ;
#8874 = CARTESIAN_POINT ( 'NONE',  ( -8.379073922441706732E-07, 4.293833316950179224, 0.3119999999988748440 ) ) ;
#8875 = DIRECTION ( 'NONE',  ( 0.000000000000000000, -0.9961946980917454342, 0.08715574274765833240 ) ) ;
#8876 = CARTESIAN_POINT ( 'NONE',  ( 0.1294417382415924134, 0.3124999999999999445, 0.3209722222222258226 ) ) ;
#8877 = CARTESIAN_POINT ( 'NONE',  ( 0.3119999999999999996, 4.748694444444444329, -0.1292346314604056745 ) ) ;
#8878 = CARTESIAN_POINT ( 'NONE',  ( 0.08598857743947876942, 5.201362809669102027, 0.2716196834644542535 ) ) ;
#8879 = CARTESIAN_POINT ( 'NONE',  ( -0.2819296736111110424, 3.967444444520310309, 0.1167790944451424923 ) ) ;
#8880 = CARTESIAN_POINT ( 'NONE',  ( 0.2819296736111110979, 3.783416666742532186, -3.452642723725051716E-17 ) ) ;
#8881 = EDGE_CURVE ( 'NONE', #1686, #2709, #20466, .T. ) ;
#8882 = CARTESIAN_POINT ( 'NONE',  ( -0.2472135954999579444, 0.2107142857142856318, -0.3402603233408160732 ) ) ;
#8883 = APPLICATION_CONTEXT ( 'configuration controlled 3d designs of mechanical parts and assemblies' ) ;
#8884 = DIRECTION ( 'NONE',  ( -0.000000000000000000, -1.000000000000000000, -0.000000000000000000 ) ) ;
#8885 = B_SPLINE_CURVE_WITH_KNOTS ( 'NONE', 3,
 ( #20491, #3787, #11231, #1953, #16837, #121, #7564, #6450, #12206, #13674, #8515, #17791, #8274, #21449, #13781, #15840, #2677, #22914, #846, #21331, #17672, #17552 ),
 .UNSPECIFIED., .F., .F.,
 ( 4, 2, 2, 2, 2, 2, 2, 2, 2, 2, 4 ),
 ( 0.000000000000000000, 0.001811609990388479826, 0.003623219980776959653, 0.004529024975971198373, 0.005434829971165437527, 0.007246439961553915836, 0.009058049951942395012, 0.009963854947136637635, 0.01086965994233087852, 0.01268126993271936377, 0.01449287992310785075 ),
 .UNSPECIFIED. ) ;
#8886 = CARTESIAN_POINT ( 'NONE',  ( -0.1167790944451423535, 4.529944444520309865, 0.2819296736111110424 ) ) ;
#8887 = CARTESIAN_POINT ( 'NONE',  ( -0.005371487263433293718, 4.488432277541713589, -0.3120000000213787317 ) ) ;
#8888 = VECTOR ( 'NONE', #5921, 39.37007874015748143 ) ;
#8889 = EDGE_CURVE ( 'NONE', #11906, #12731, #22567, .T. ) ;
#8890 = DATE_AND_TIME ( #21810, #18115 ) ;
#8891 = CARTESIAN_POINT ( 'NONE',  ( 0.1292346314604056745, 0.08402777777777743762, -0.3119999999999999996 ) ) ;
#8892 = CARTESIAN_POINT ( 'NONE',  ( -0.2764156081756484196, 1.692557448933383907E-17, 0.3105555555555591929 ) ) ;
#8893 = CARTESIAN_POINT ( 'NONE',  ( -0.2819296736111110979, 4.088972222298088433, 0.000000000000000000 ) ) ;
#8894 = CARTESIAN_POINT ( 'NONE',  ( -0.2704625092236399575, 4.840203190926620103, 0.1611498159692242860 ) ) ;
#8895 = CARTESIAN_POINT ( 'NONE',  ( -0.08164014826675215775, 4.458214446043974100, 0.3038864024473010295 ) ) ;
#8896 = CARTESIAN_POINT ( 'NONE',  ( 0.3003475124358242487, 3.066692553488282957, 3.638968604327563749 ) ) ;
#8897 = CARTESIAN_POINT ( 'NONE',  ( 0.2923287055106771337, 0.09017857133102899492, -0.2123892367102620249 ) ) ;
#8898 = CARTESIAN_POINT ( 'NONE',  ( -0.2819296736111110979, 0.3409722221463556413, -3.452642723725051716E-17 ) ) ;
#8899 = CARTESIAN_POINT ( 'NONE',  ( 0.4687500000000002220, 0.2150860547839004433, 0.05816278416816413055 ) ) ;
#8900 = FACE_OUTER_BOUND ( 'NONE', #9684, .T. ) ;
#8901 = CARTESIAN_POINT ( 'NONE',  ( -0.1566782819544844385, 0.2231665291434455078, -0.7334692270860763141 ) ) ;
#8902 = CARTESIAN_POINT ( 'NONE',  ( -0.1954553509668046918, -0.1954553509668046640, -0.01583333333333228690 ) ) ;
#8903 = CARTESIAN_POINT ( 'NONE',  ( -3.385114897866767815E-17, -0.2764156081756484196, 0.05361111111111271227 ) ) ;
#8904 = B_SPLINE_CURVE_WITH_KNOTS ( 'NONE', 3,
 ( #21062, #22768, #218, #2050, #3880, #16923, #2296, #2179, #7656, #15106, #9612, #17042, #6662, #19467, #2765, #10218, #21181, #16057, #17522, #17642, #23472, #4596, #930, #12054, #8361, #818, #6784, #10100, #14107, #23111, #15697, #21537, #14227, #12177, #13756, #1057, #19585, #1179, #8617, #15811, #15928, #23231, #6541, #21303, #8244, #12294, #8485, #4471, #21661, #19353, #11936, #4824, #2877, #6421, #13874 ),
 .UNSPECIFIED., .F., .F.,
 ( 4, 2, 1, 1, 1, 1, 2, 2, 2, 2, 2, 2, 1, 1, 2, 2, 1, 1, 1, 2, 2, 2, 2, 2, 2, 2, 2, 1, 1, 2, 2, 1, 1, 4 ),
 ( 0.1553377600788464485, 0.1553555988096145257, 0.1553734375403825752, 0.1554091150019187018, 0.1554804699249909827, 0.1556231797711355169, 0.1559085994634245853, 0.1564794388480027221, 0.1576211176171589956, 0.1599044751554715427, 0.1621878326937841175, 0.1644711902320966646, 0.1647566099243857329, 0.1648993197705302671, 0.1649706746936025481, 0.1649795940589865728, 0.1649885134243705975, 0.1650063521551386470, 0.1650420296166747458, 0.1656128690012524107, 0.1667545477704077406, 0.1678962265395630704, 0.1690379053087184003, 0.1701795840778737301, 0.1713212628470290599, 0.1718921022316067249, 0.1721775219238955712, 0.1723202317700399944, 0.1723915866931121921, 0.1724272641546482909, 0.1724361835200323156, 0.1724451028854163404, 0.1724629416161844175, 0.1736046203853397751 ),
 .UNSPECIFIED. ) ;
#8905 = ORIENTED_EDGE ( 'NONE', *, *, #13080, .T. ) ;
#8906 = ORIENTED_EDGE ( 'NONE', *, *, #19643, .T. ) ;
#8907 = CARTESIAN_POINT ( 'NONE',  ( -0.1236067977499789583, 0.06428571428571425161, -0.3804226065180614791 ) ) ;
#8908 = CARTESIAN_POINT ( 'NONE',  ( -0.08166536455864450983, 3.847164242900631859, 0.3038794701439369583 ) ) ;
#8909 = CARTESIAN_POINT ( 'NONE',  ( -0.2206173157302028787, 0.1083333333333329901, 0.2206173157302027954 ) ) ;
#8910 = CARTESIAN_POINT ( 'NONE',  ( -0.1167790944451423535, 3.821611111186977272, 0.2819296736111110424 ) ) ;
#8911 = VECTOR ( 'NONE', #16044, 39.37007874015748143 ) ;
#8912 = CARTESIAN_POINT ( 'NONE',  ( -0.2923287055106771337, 0.1116071427596004445, -0.2123892367102620804 ) ) ;
#8913 = EDGE_LOOP ( 'NONE', ( #18714, #19832, #8137, #20681 ) ) ;
#8914 = CARTESIAN_POINT ( 'NONE',  ( -0.1993543840281266355, 4.484805555631421470, 0.1993543840281267465 ) ) ;
#8915 = EDGE_CURVE ( 'NONE', #10834, #17381, #3077, .T. ) ;
#8916 = CARTESIAN_POINT ( 'NONE',  ( 0.000000000000000000, 3.700000000000000622, 0.000000000000000000 ) ) ;
#8917 = PLANE ( 'NONE',  #9493 ) ;
#8918 = EDGE_LOOP ( 'NONE', ( #7736, #19724, #651, #18973 ) ) ;
#8919 = CARTESIAN_POINT ( 'NONE',  ( 0.2818991764556534885, 4.359328379276062648, 0.1340068449377857795 ) ) ;
#8920 = CARTESIAN_POINT ( 'NONE',  ( -0.2819296736111110979, 5.241750000075865223, 0.000000000000000000 ) ) ;
#8921 = CARTESIAN_POINT ( 'NONE',  ( 0.0002807800906013602411, 4.210492038945215398, -0.3119999059963255994 ) ) ;
#8922 = CARTESIAN_POINT ( 'NONE',  ( 0.2977072594216367274, -5.468793635004571549E-17, -0.08687392608830331320 ) ) ;
#8923 = AXIS2_PLACEMENT_3D ( 'NONE', #5706, #9611, #6390 ) ;
#8924 = CARTESIAN_POINT ( 'NONE',  ( -0.2819296736111110424, 4.911888888964754507, 0.1167790944451424923 ) ) ;
#8925 = APPROVAL_ROLE ( '' ) ;
#8926 = CARTESIAN_POINT ( 'NONE',  ( -0.4692113125120477846, 0.2611562006105974665, 0.04763592618481432561 ) ) ;
#8927 = ORIENTED_EDGE ( 'NONE', *, *, #3638, .T. ) ;
#8928 = CARTESIAN_POINT ( 'NONE',  ( 0.1993543840281266355, 0.2645833332574666907, 0.1993543840281267465 ) ) ;
#8929 = EDGE_LOOP ( 'NONE', ( #8958, #12524, #7489, #14752 ) ) ;
#8930 = CARTESIAN_POINT ( 'NONE',  ( -5.178964085587577574E-17, 0.03541666659080003332, 0.2819296736111110979 ) ) ;
#8931 = DIRECTION ( 'NONE',  ( -1.000000000000000000, 0.000000000000000000, 0.000000000000000000 ) ) ;
#8932 = PLANE ( 'NONE',  #17168 ) ;
#8933 = CARTESIAN_POINT ( 'NONE',  ( -0.1236067977499789583, -0.07857142857142858372, -0.3804226065180614791 ) ) ;
#8934 = CYLINDRICAL_SURFACE ( 'NONE', #24081, 0.4000000000000000222 ) ;
#8935 = CARTESIAN_POINT ( 'NONE',  ( 0.3003475124358450099, 4.111524471938507119, -3.730379552481990491 ) ) ;
#8936 = PLANE ( 'NONE',  #18309 ) ;
#8937 = CARTESIAN_POINT ( 'NONE',  ( 0.1993543840281266910, 0.09791666659080001944, -0.1993543840281266910 ) ) ;
#8938 = CARTESIAN_POINT ( 'NONE',  ( -0.2819296736111110424, 4.425777777853643791, 0.1167790944451424923 ) ) ;
#8939 = DIRECTION ( 'NONE',  ( 0.000000000000000000, 0.000000000000000000, -1.000000000000000000 ) ) ;
#8940 = CARTESIAN_POINT ( 'NONE',  ( 0.2982715858037333079, 4.532666993397491240, -0.09547612790609734390 ) ) ;
#8941 = CARTESIAN_POINT ( 'NONE',  ( 0.2819296736111110979, 5.005638888964754507, -3.452642723725051716E-17 ) ) ;
#8942 = ADVANCED_FACE ( 'NONE', ( #16210 ), #20228, .T. ) ;
#8943 = CARTESIAN_POINT ( 'NONE',  ( -0.1338711291748117538, 0.04577227553858571885, -0.2639161900088024537 ) ) ;
#8944 = CARTESIAN_POINT ( 'NONE',  ( 0.01475392317844165246, 3.765650153564859437, -0.3120907002652242856 ) ) ;
#8945 = CARTESIAN_POINT ( 'NONE',  ( 3.820898013339742174E-17, 5.384999999999999787, 0.3119999999999999996 ) ) ;
#8946 = CARTESIAN_POINT ( 'NONE',  ( 0.2938106225197735233, 3.922092824913935072, -0.1134682388069244707 ) ) ;
#8947 = CARTESIAN_POINT ( 'NONE',  ( -0.3119999999999999996, 4.387583333485066461, -0.1292346314604056468 ) ) ;
#8948 = CARTESIAN_POINT ( 'NONE',  ( -0.1167790944451423119, 4.467444444520309865, -0.2819296736111110979 ) ) ;
#8949 = CARTESIAN_POINT ( 'NONE',  ( 0.2819296736111110424, 3.939666666742531742, -0.1167790944451423396 ) ) ;
#8950 = ORIENTED_EDGE ( 'NONE', *, *, #11311, .T. ) ;
#8951 = PRODUCT_DEFINITION_SHAPE ( 'NONE', 'NONE',  #19252 ) ;
#8952 = VERTEX_POINT ( 'NONE', #23993 ) ;
#8953 = ORIENTED_EDGE ( 'NONE', *, *, #15132, .F. ) ;
#8954 = APPROVAL_ROLE ( '' ) ;
#8955 = CIRCLE ( 'NONE', #8216, 0.7500000000000001110 ) ;
#8956 = CARTESIAN_POINT ( 'NONE',  ( -0.3039946847935154350, 4.944401201872332230, -0.08125663725904756773 ) ) ;
#8957 = CARTESIAN_POINT ( 'NONE',  ( -0.5116234456863258950, 1.828961980248579033, -2.721610195421419576 ) ) ;
#8958 = ORIENTED_EDGE ( 'NONE', *, *, #13984, .F. ) ;
#8959 = CARTESIAN_POINT ( 'NONE',  ( -0.1292346314604056190, 0.3618055554038225874, -0.3119999999999999996 ) ) ;
#8960 = CIRCLE ( 'NONE', #1937, 0.7500000000000001110 ) ;
#8961 = CARTESIAN_POINT ( 'NONE',  ( -0.2704070349950395968, 4.395731272337639162, 0.1569688776948623132 ) ) ;
#8962 = CARTESIAN_POINT ( 'NONE',  ( -0.2515410393475099315, 5.120907854582883445, 0.1785482678038019244 ) ) ;
#8963 = DIRECTION ( 'NONE',  ( -0.000000000000000000, -1.000000000000000000, -0.000000000000000000 ) ) ;
#8964 = CARTESIAN_POINT ( 'NONE',  ( -7.000945310522701902E-17, 0.3821428571428570620, 0.3999999999999999667 ) ) ;
#8965 = VERTEX_POINT ( 'NONE', #16328 ) ;
#8966 = CARTESIAN_POINT ( 'NONE',  ( 0.3057358687413568865, 5.087467270640830819, -0.06349570009324533026 ) ) ;
#8967 = CARTESIAN_POINT ( 'NONE',  ( 0.2764156081756483641, 0.1144950937579610056, 0.2862500000000035016 ) ) ;
#8968 = CARTESIAN_POINT ( 'NONE',  ( -0.2819296736111110424, 4.127166666742532186, -0.1167790944451423119 ) ) ;
#8969 = CARTESIAN_POINT ( 'NONE',  ( 0.2819296736111110979, 5.161888888964753619, -0.1167790944451423396 ) ) ;
#8970 = B_SPLINE_CURVE_WITH_KNOTS ( 'NONE', 3,
 ( #16801, #8994, #3620, #3502, #22277, #14610 ),
 .UNSPECIFIED., .F., .F.,
 ( 4, 2, 4 ),
 ( 0.000000000000000000, 0.003274885914386082859, 0.006549771828772165717 ),
 .UNSPECIFIED. ) ;
#8971 = CARTESIAN_POINT ( 'NONE',  ( -0.07990078027836888808, -0.4951351403630674386, 0.4110703004652378478 ) ) ;
#8972 = CARTESIAN_POINT ( 'NONE',  ( -0.03683881386148459003, 4.237268085405634821, 0.3098358431719507866 ) ) ;
#8973 = CARTESIAN_POINT ( 'NONE',  ( 0.1292346314604056190, 4.144527777777777366, -0.3119999999999999996 ) ) ;
#8974 = CARTESIAN_POINT ( 'NONE',  ( 0.1292346314604058410, 4.908416666818398610, 0.3119999999999998885 ) ) ;
#8975 = CARTESIAN_POINT ( 'NONE',  ( -0.2819296736111110979, 5.088972222298087544, 0.000000000000000000 ) ) ;
#8976 = VECTOR ( 'NONE', #22670, 39.37007874015748143 ) ;
#8977 = AXIS2_PLACEMENT_3D ( 'NONE', #21821, #1227, #8653 ) ;
#8978 = CARTESIAN_POINT ( 'NONE',  ( 0.2206173157302028787, 4.849388888888888083, 0.2206173157302027954 ) ) ;
#8979 = ORIENTED_EDGE ( 'NONE', *, *, #12124, .F. ) ;
#8980 = CARTESIAN_POINT ( 'NONE',  ( 5.253288188650943643E-17, 5.197747365142496356, 0.2859756893339090444 ) ) ;
#8981 = CARTESIAN_POINT ( 'NONE',  ( -0.1570247121346943220, 4.900413900555340874, 0.2726770930307582663 ) ) ;
#8982 = ORIENTED_EDGE ( 'NONE', *, *, #5678, .F. ) ;
#8983 =( BOUNDED_SURFACE ( )  B_SPLINE_SURFACE ( 1, 2, ( 
 ( #15384, #12338, #3407, #4989, #16098, #19755, #3282, #14513, #20116, #21464, #16340, #1462, #23512, #5107, #21577, #23635, #10497, #6585, #8649, #12453, #1340, #14391, #21934, #5227, #23396, #4872, #21817, #3050, #6703, #6828, #19872, #6952, #17927, #18165, #1223, #12573, #19994, #14148, #10857, #4748, #12701, #979, #8897, #8406, #8770, #10736, #1099, #14268, #23753, #7075, #21705, #3164, #15856, #10614, #18044, #16222, #23273, #14034, #12219, #19629, #2927, #10386, #17808, #8531, #15975, #5479, #15119, #9019, #7433, #16935, #233, #2060, #13299, #18524, #11215, #24001, #16460, #12944, #7313, #1813, #14763, #9258, #12820, #22545, #5354, #22421, #1698, #10979, #5722, #20714, #13059, #18285, #18644, #5594, #7668, #16699, #20356, #1936, #14880, #9501, #3528, #5835, #1583, #4010, #11093, #23872, #13182, #24118, #9384, #7192, #22297, #20477, #20595, #18405, #22178, #20238, #14637, #3646, #22059, #3772, #16824, #106, #9135, #3890, #7547, #14999, #16580, #11336, #18765, #13539, #4126, #18891, #20954, #22780, #9869, #17296, #6192, #21073, #17182, #22898, #710 ),
 ( #2662, #13657, #17536, #8021, #4248, #6074, #8258, #2192, #589, #10112, #829, #19363, #6433, #11699, #4363, #468, #9623, #19123, #7899, #2427, #15351, #15471, #5952, #15708, #22663, #15588, #19012, #11582, #23012, #13887, #11821, #11458, #19240, #2544, #23122, #9992, #17416, #8138, #6314, #21314, #20834, #17056, #349, #7789, #13766, #15234, #13411, #21192, #4483, #11950, #2308, #9745, #3137, #23721, #1435, #21547, #8498, #14118, #10226, #17654, #23605, #3252, #10468, #15822, #17774, #21673, #4958, #15938, #16069, #23363, #7045, #8624, #19718, #6673, #6919, #18138, #14482, #941, #19965, #5076, #3020, #8736, #1067, #10587, #4836, #8371, #8864, #23241, #12304, #16308, #14358, #6550, #23481, #12425, #19595, #17897, #6798, #1312, #14236, #16192, #19838, #21788, #1191, #2774, #18014, #4605, #14000, #12067, #12545, #19480, #10703, #2890, #21433, #10350, #4718, #12191, #5568, #7643, #12667, #16794, #13033, #20210, #7284, #23843, #14734, #24095, #201, #16433, #12790, #7405, #18494, #16552, #20087, #16906, #5196, #9474, #9102, #7163, #3745, #12912, #23973 ) ),
 .UNSPECIFIED., .F., .F., .T. ) 
 B_SPLINE_SURFACE_WITH_KNOTS ( ( 2, 2 ),
 ( 3, 2, 2, 2, 2, 2, 2, 2, 2, 2, 2, 2, 2, 2, 2, 2, 2, 2, 2, 2, 2, 2, 2, 2, 2, 2, 2, 2, 2, 2, 2, 2, 2, 2, 2, 2, 2, 2, 2, 2, 2, 2, 2, 2, 2, 2, 2, 2, 2, 2, 2, 2, 2, 2, 2, 2, 2, 2, 2, 2, 2, 2, 2, 2, 2, 2, 2, 2, 2, 2, 3 ),
 ( 0.000000000000000000, 1.000000000000000000 ),
 ( 0.000000000000000000, 0.01428571428571428527, 0.02857142857142857054, 0.04285714285714285754, 0.05714285714285714107, 0.07142857142857142461, 0.08571428571428571508, 0.1000000000000000056, 0.1142857142857142821, 0.1285714285714285587, 0.1428571428571428492, 0.1571428571428571397, 0.1714285714285714302, 0.1857142857142857206, 0.2000000000000000111, 0.2142857142857142738, 0.2285714285714285643, 0.2428571428571428548, 0.2571428571428571175, 0.2714285714285714080, 0.2857142857142856984, 0.2999999999999999889, 0.3142857142857142794, 0.3285714285714285698, 0.3428571428571428603, 0.3571428571428571508, 0.3714285714285714413, 0.3857142857142857317, 0.4000000000000000222, 0.4142857142857143127, 0.4285714285714285476, 0.4428571428571428381, 0.4571428571428571286, 0.4714285714285714191, 0.4857142857142857095, 0.5000000000000000000, 0.5142857142857142350, 0.5285714285714285809, 0.5428571428571428159, 0.5571428571428571619, 0.5714285714285713969, 0.5857142857142857428, 0.5999999999999999778, 0.6142857142857143238, 0.6285714285714285587, 0.6428571428571429047, 0.6571428571428571397, 0.6714285714285713746, 0.6857142857142857206, 0.6999999999999999556, 0.7142857142857143016, 0.7285714285714285365, 0.7428571428571428825, 0.7571428571428571175, 0.7714285714285714635, 0.7857142857142856984, 0.8000000000000000444, 0.8142857142857142794, 0.8285714285714286254, 0.8428571428571428603, 0.8571428571428570953, 0.8714285714285714413, 0.8857142857142856762, 0.9000000000000000222, 0.9142857142857142572, 0.9285714285714286031, 0.9428571428571428381, 0.9571428571428571841, 0.9714285714285714191, 0.9857142857142857650, 1.000000000000000000 ),
 .UNSPECIFIED. ) 
 GEOMETRIC_REPRESENTATION_ITEM ( )  RATIONAL_B_SPLINE_SURFACE ( (
 ( 1.000000000000000000, 0.9510565162951535312, 1.000000000000000000, 0.9510565162951535312, 1.000000000000000000, 0.9510565162951535312, 1.000000000000000000, 0.9510565162951535312, 1.000000000000000000, 0.9510565162951535312, 1.000000000000000000, 0.9510565162951535312, 1.000000000000000000, 0.9510565162951535312, 1.000000000000000000, 0.9510565162951535312, 1.000000000000000000, 0.9510565162951535312, 1.000000000000000000, 0.9510565162951535312, 1.000000000000000000, 0.9510565162951535312, 1.000000000000000000, 0.9510565162951535312, 1.000000000000000000, 0.9510565162951535312, 1.000000000000000000, 0.9510565162951535312, 1.000000000000000000, 0.9510565162951535312, 1.000000000000000000, 0.9510565162951535312, 1.000000000000000000, 0.9510565162951535312, 1.000000000000000000, 0.9510565162951535312, 1.000000000000000000, 0.9510565162951535312, 1.000000000000000000, 0.9510565162951535312, 1.000000000000000000, 0.9510565162951535312, 1.000000000000000000, 0.9510565162951535312, 1.000000000000000000, 0.9510565162951535312, 1.000000000000000000, 0.9510565162951535312, 1.000000000000000000, 0.9510565162951535312, 1.000000000000000000, 0.9510565162951535312, 1.000000000000000000, 0.9510565162951535312, 1.000000000000000000, 0.9510565162951535312, 1.000000000000000000, 0.9510565162951535312, 1.000000000000000000, 0.9510565162951535312, 1.000000000000000000, 0.9510565162951535312, 1.000000000000000000, 0.9510565162951535312, 1.000000000000000000, 0.9510565162951535312, 1.000000000000000000, 0.9510565162951535312, 1.000000000000000000, 0.9510565162951535312, 1.000000000000000000, 0.9510565162951535312, 1.000000000000000000, 0.9510565162951535312, 1.000000000000000000, 0.9510565162951535312, 1.000000000000000000, 0.9510565162951535312, 1.000000000000000000, 0.9510565162951535312, 1.000000000000000000, 0.9510565162951535312, 1.000000000000000000, 0.9510565162951535312, 1.000000000000000000, 0.9510565162951535312, 1.000000000000000000, 0.9510565162951535312, 1.000000000000000000, 0.9510565162951535312, 1.000000000000000000, 0.9510565162951535312, 1.000000000000000000, 0.9510565162951535312, 1.000000000000000000, 0.9510565162951535312, 1.000000000000000000, 0.9510565162951535312, 1.000000000000000000, 0.9510565162951535312, 1.000000000000000000, 0.9510565162951535312, 1.000000000000000000, 0.9510565162951535312, 1.000000000000000000, 0.9510565162951535312, 1.000000000000000000, 0.9510565162951535312, 1.000000000000000000, 0.9510565162951535312, 1.000000000000000000, 0.9510565162951535312, 1.000000000000000000, 0.9510565162951535312, 1.000000000000000000, 0.9510565162951535312, 1.000000000000000000, 0.9510565162951535312, 1.000000000000000000, 0.9510565162951535312, 1.000000000000000000, 0.9510565162951535312, 1.000000000000000000, 0.9510565162951535312, 1.000000000000000000, 0.9510565162951535312, 1.000000000000000000, 0.9510565162951535312, 1.000000000000000000, 0.9510565162951535312, 1.000000000000000000, 0.9510565162951535312, 1.000000000000000000, 0.9510565162951535312, 1.000000000000000000, 0.9510565162951535312, 1.000000000000000000, 0.9510565162951535312, 1.000000000000000000, 0.9510565162951535312, 1.000000000000000000),
 ( 1.000000000000000000, 0.9510565162951535312, 1.000000000000000000, 0.9510565162951535312, 1.000000000000000000, 0.9510565162951535312, 1.000000000000000000, 0.9510565162951535312, 1.000000000000000000, 0.9510565162951535312, 1.000000000000000000, 0.9510565162951535312, 1.000000000000000000, 0.9510565162951535312, 1.000000000000000000, 0.9510565162951535312, 1.000000000000000000, 0.9510565162951535312, 1.000000000000000000, 0.9510565162951535312, 1.000000000000000000, 0.9510565162951535312, 1.000000000000000000, 0.9510565162951535312, 1.000000000000000000, 0.9510565162951535312, 1.000000000000000000, 0.9510565162951535312, 1.000000000000000000, 0.9510565162951535312, 1.000000000000000000, 0.9510565162951535312, 1.000000000000000000, 0.9510565162951535312, 1.000000000000000000, 0.9510565162951535312, 1.000000000000000000, 0.9510565162951535312, 1.000000000000000000, 0.9510565162951535312, 1.000000000000000000, 0.9510565162951535312, 1.000000000000000000, 0.9510565162951535312, 1.000000000000000000, 0.9510565162951535312, 1.000000000000000000, 0.9510565162951535312, 1.000000000000000000, 0.9510565162951535312, 1.000000000000000000, 0.9510565162951535312, 1.000000000000000000, 0.9510565162951535312, 1.000000000000000000, 0.9510565162951535312, 1.000000000000000000, 0.9510565162951535312, 1.000000000000000000, 0.9510565162951535312, 1.000000000000000000, 0.9510565162951535312, 1.000000000000000000, 0.9510565162951535312, 1.000000000000000000, 0.9510565162951535312, 1.000000000000000000, 0.9510565162951535312, 1.000000000000000000, 0.9510565162951535312, 1.000000000000000000, 0.9510565162951535312, 1.000000000000000000, 0.9510565162951535312, 1.000000000000000000, 0.9510565162951535312, 1.000000000000000000, 0.9510565162951535312, 1.000000000000000000, 0.9510565162951535312, 1.000000000000000000, 0.9510565162951535312, 1.000000000000000000, 0.9510565162951535312, 1.000000000000000000, 0.9510565162951535312, 1.000000000000000000, 0.9510565162951535312, 1.000000000000000000, 0.9510565162951535312, 1.000000000000000000, 0.9510565162951535312, 1.000000000000000000, 0.9510565162951535312, 1.000000000000000000, 0.9510565162951535312, 1.000000000000000000, 0.9510565162951535312, 1.000000000000000000, 0.9510565162951535312, 1.000000000000000000, 0.9510565162951535312, 1.000000000000000000, 0.9510565162951535312, 1.000000000000000000, 0.9510565162951535312, 1.000000000000000000, 0.9510565162951535312, 1.000000000000000000, 0.9510565162951535312, 1.000000000000000000, 0.9510565162951535312, 1.000000000000000000, 0.9510565162951535312, 1.000000000000000000, 0.9510565162951535312, 1.000000000000000000, 0.9510565162951535312, 1.000000000000000000, 0.9510565162951535312, 1.000000000000000000, 0.9510565162951535312, 1.000000000000000000, 0.9510565162951535312, 1.000000000000000000, 0.9510565162951535312, 1.000000000000000000, 0.9510565162951535312, 1.000000000000000000, 0.9510565162951535312, 1.000000000000000000, 0.9510565162951535312, 1.000000000000000000, 0.9510565162951535312, 1.000000000000000000, 0.9510565162951535312, 1.000000000000000000, 0.9510565162951535312, 1.000000000000000000, 0.9510565162951535312, 1.000000000000000000) ) ) 
 REPRESENTATION_ITEM ( '' )  SURFACE ( )  );
#8984 = CARTESIAN_POINT ( 'NONE',  ( 0.1306872919485616846, 0.3155070326520292290, 0.2706250000000035016 ) ) ;
#8985 = CARTESIAN_POINT ( 'NONE',  ( -0.2233192592356399442, 0.3937499999024575148, -0.3073725909049500049 ) ) ;
#8986 =( BOUNDED_CURVE ( )  B_SPLINE_CURVE ( 2, ( #10042, #17231, #13464, #7834, #17464, #2107, #513, #19291, #756 ),
 .UNSPECIFIED., .F., .F. ) 
 B_SPLINE_CURVE_WITH_KNOTS ( ( 3, 2, 2, 2, 3 ),
 ( 0.5208333333333334814, 0.5312500000000001110, 0.5416666666666667407, 0.5520833333333334814, 0.5625000000000001110 ),
 .UNSPECIFIED. ) 
 CURVE ( )  GEOMETRIC_REPRESENTATION_ITEM ( )  RATIONAL_B_SPLINE_CURVE ( ( 0.9999999999999992228, 0.9238795325112875156, 1.000000000000000000, 0.9238795325112867385, 1.000000000000000000, 0.9238795325112867385, 1.000000000000000000, 0.9238795325112859613, 1.000000000000000888 ) ) 
 REPRESENTATION_ITEM ( '' )  );
#8987 = CARTESIAN_POINT ( 'NONE',  ( 0.3236067977499789694, 0.03571428571428568455, 0.2351141009169893659 ) ) ;
#8988 = ADVANCED_FACE ( 'NONE', ( #5469 ), #22945, .F. ) ;
#8989 = DIRECTION ( 'NONE',  ( 0.8660254037844437036, 0.000000000000000000, 0.4999999999999910627 ) ) ;
#8990 = AXIS2_PLACEMENT_3D ( 'NONE', #7338, #20266, #22087 ) ;
#8991 = CARTESIAN_POINT ( 'NONE',  ( 0.1993543840281266910, 0.3340277777019111660, -0.1993543840281266910 ) ) ;
#8992 = CARTESIAN_POINT ( 'NONE',  ( 0.1144950937579611444, 0.2764156081756483641, 0.3556944444444484210 ) ) ;
#8993 = CARTESIAN_POINT ( 'NONE',  ( -0.1993543840281266910, 5.137583333409199149, -0.1993543840281266910 ) ) ;
#8994 = CARTESIAN_POINT ( 'NONE',  ( -0.4802530987341848134, -0.2139104309994724062, 0.05348414072159345806 ) ) ;
#8995 = ORIENTED_EDGE ( 'NONE', *, *, #16334, .T. ) ;
#8996 = CARTESIAN_POINT ( 'NONE',  ( -0.2819296736111110979, 4.797305555631420582, 0.000000000000000000 ) ) ;
#8997 = CARTESIAN_POINT ( 'NONE',  ( -0.1003379275823265415, 4.179873057794735836, 0.2961323726520993516 ) ) ;
#8998 = DIRECTION ( 'NONE',  ( -0.000000000000000000, -1.000000000000000000, -0.000000000000000000 ) ) ;
#8999 = CARTESIAN_POINT ( 'NONE',  ( 0.2206173157302028232, 0.5736111109593782231, -0.2206173157302028232 ) ) ;
#9000 = CARTESIAN_POINT ( 'NONE',  ( 0.1292346314604058410, 4.790361111111110404, 0.3119999999999998885 ) ) ;
#9001 = CARTESIAN_POINT ( 'NONE',  ( 0.1167790944451422702, 4.057722222298087544, -0.2819296736111110979 ) ) ;
#9002 = CARTESIAN_POINT ( 'NONE',  ( 5.178964085587577574E-17, 3.769527777853644235, 0.2819296736111110979 ) ) ;
#9003 = CARTESIAN_POINT ( 'NONE',  ( 7.459700445346810805E-07, 4.043833313442511290, -0.3119999999991081574 ) ) ;
#9004 = CARTESIAN_POINT ( 'NONE',  ( -1.910449006669871087E-17, 4.425777777777777366, -0.3119999999999999996 ) ) ;
#9005 = ORIENTED_EDGE ( 'NONE', *, *, #2055, .T. ) ;
#9006 = DIRECTION ( 'NONE',  ( -0.000000000000000000, -0.000000000000000000, -1.000000000000000000 ) ) ;
#9007 = ORIENTED_EDGE ( 'NONE', *, *, #22555, .T. ) ;
#9008 = CARTESIAN_POINT ( 'NONE',  ( 0.2819296736111110979, 4.266055555631421470, 0.1167790944451422425 ) ) ;
#9009 = CARTESIAN_POINT ( 'NONE',  ( -0.2025260695160075453, 4.494500837587061426, -0.2412900599587802508 ) ) ;
#9010 = EDGE_CURVE ( 'NONE', #1106, #16767, #7283, .T. ) ;
#9011 = ADVANCED_FACE ( 'NONE', ( #4117 ), #15226, .T. ) ;
#9012 = CARTESIAN_POINT ( 'NONE',  ( 1.910449006669871087E-17, 0.08749999999999966138, -0.3119999999999999996 ) ) ;
#9013 = CARTESIAN_POINT ( 'NONE',  ( 0.1144950937579611444, 0.2764156081756483641, 0.3487500000000040012 ) ) ;
#9014 = CARTESIAN_POINT ( 'NONE',  ( 0.1993543840281267465, 3.776472222298087988, 0.1993543840281266633 ) ) ;
#9015 = CARTESIAN_POINT ( 'NONE',  ( -0.04084070934671252956, 3.959337429128877872, 0.3120000006064171938 ) ) ;
#9016 = EDGE_CURVE ( 'NONE', #1241, #16785, #15464, .T. ) ;
#9017 = CARTESIAN_POINT ( 'NONE',  ( 1.910449006669871087E-17, 0.5249999998482670627, -0.3119999999999999996 ) ) ;
#9018 = CARTESIAN_POINT ( 'NONE',  ( 0.2782497666485165277, 0.06249891821425377497, 0.1411420113220940853 ) ) ;
#9019 = CARTESIAN_POINT ( 'NONE',  ( -0.2233192592356399442, 0.1794642856167432965, -0.3073725909049500049 ) ) ;
#9020 = CARTESIAN_POINT ( 'NONE',  ( -0.1167790944451424368, 0.3513888888130222155, 0.2819296736111110424 ) ) ;
#9021 = CARTESIAN_POINT ( 'NONE',  ( 0.4805070082343983473, -0.2560807851245830435, 0.04413116910601663084 ) ) ;
#9022 = CARTESIAN_POINT ( 'NONE',  ( 0.3999999999999999667, 0.03749999980491518919, -0.1299678784931625197 ) ) ;
#9023 = CARTESIAN_POINT ( 'NONE',  ( -0.1419325426031897985, 0.2081706596913604768, -0.7365160675939218526 ) ) ;
#9024 = CARTESIAN_POINT ( 'NONE',  ( -0.1954553509668046640, 0.1954553509668046918, 0.02583333333333472440 ) ) ;
#9025 = CARTESIAN_POINT ( 'NONE',  ( -0.1954553509668046918, -0.1954553509668046640, -0.1199999999999998013 ) ) ;
#9026 = ORIENTED_EDGE ( 'NONE', *, *, #17176, .F. ) ;
#9027 = VERTEX_POINT ( 'NONE', #19001 ) ;
#9028 = CARTESIAN_POINT ( 'NONE',  ( -0.3616234456863465230, 3.514980167629567998, 2.635972749958888528 ) ) ;
#9029 = LINE ( 'NONE', #23882, #2969 ) ;
#9030 = CARTESIAN_POINT ( 'NONE',  ( -0.3119999999999999996, 0.04930555555555521385, 0.1292346314604056190 ) ) ;
#9031 = CARTESIAN_POINT ( 'NONE',  ( 0.1167790944451422702, 3.849388888964754951, -0.2819296736111110424 ) ) ;
#9032 = CARTESIAN_POINT ( 'NONE',  ( -0.3613381517857143232, 0.1866071427596003862, -0.1174058825155741004 ) ) ;
#9033 = ORIENTED_EDGE ( 'NONE', *, *, #22131, .T. ) ;
#9034 = CARTESIAN_POINT ( 'NONE',  ( -1.726321361862525858E-17, 4.519527777853643791, -0.2819296736111110979 ) ) ;
#9035 = CARTESIAN_POINT ( 'NONE',  ( 1.910449006669871087E-17, 0.1361111109593781676, -0.3119999999999999996 ) ) ;
#9036 = CARTESIAN_POINT ( 'NONE',  ( -0.3120000000000000551, 0.1534722220704892726, 0.1292346314604056190 ) ) ;
#9037 = VERTEX_POINT ( 'NONE', #460 ) ;
#9038 = CARTESIAN_POINT ( 'NONE',  ( -7.000945310522701902E-17, 0.3821428571428570620, 0.3999999999999999667 ) ) ;
#9039 = CARTESIAN_POINT ( 'NONE',  ( -1.726321361862525858E-17, 5.172305555631420582, -0.2819296736111110979 ) ) ;
#9040 = CARTESIAN_POINT ( 'NONE',  ( 0.2806972955496128130, 4.200680281449905351, -0.1374172179846145925 ) ) ;
#9041 = LINE ( 'NONE', #1485, #13494 ) ;
#9042 = CARTESIAN_POINT ( 'NONE',  ( 0.3236067977499790249, 0.1928571428571428104, -0.2351141009169892826 ) ) ;
#9043 = CARTESIAN_POINT ( 'NONE',  ( 5.178964085587577574E-17, 4.700083333409199149, 0.2819296736111110979 ) ) ;
#9044 = APPROVAL_STATUS ( 'not_yet_approved' ) ;
#9045 = DIRECTION ( 'NONE',  ( -0.7071067811865475727, -0.7071067811865475727, -0.000000000000000000 ) ) ;
#9046 = CARTESIAN_POINT ( 'NONE',  ( 2.369221741255291391, 0.000000000000000000, -1.763529041877836434 ) ) ;
#9047 = CARTESIAN_POINT ( 'NONE',  ( 1.726321361862525858E-17, 0.3409722221463556413, -0.2819296736111110979 ) ) ;
#9048 = VERTEX_POINT ( 'NONE', #6183 ) ;
#9049 = CARTESIAN_POINT ( 'NONE',  ( 0.1993543840281266355, 0.2090277777019111383, 0.1993543840281267465 ) ) ;
#9050 = CARTESIAN_POINT ( 'NONE',  ( -0.2081274754753156542, 4.716903871102764434, -0.2331404442114669018 ) ) ;
#9051 = CARTESIAN_POINT ( 'NONE',  ( -0.2485974056653872943, 5.197792025490196366, -0.1419878697022586012 ) ) ;
#9052 = CARTESIAN_POINT ( 'NONE',  ( -0.2233192592356399997, 0.3973214284738861291, 0.3073725909049499494 ) ) ;
#9053 = CARTESIAN_POINT ( 'NONE',  ( -0.2230971623002953874, 0.2230971623002954152, -0.1113194444444443598 ) ) ;
#9054 = CARTESIAN_POINT ( 'NONE',  ( -0.4875000000000003220, -0.2598076211353319009, 0.06112444011295369711 ) ) ;
#9055 = CARTESIAN_POINT ( 'NONE',  ( -0.2329574276516829245, 3.884553289494028672, -0.2088804256055948050 ) ) ;
#9056 = CARTESIAN_POINT ( 'NONE',  ( 0.1993543840281266910, 0.04236111103524448085, -0.1993543840281266910 ) ) ;
#9057 = CARTESIAN_POINT ( 'NONE',  ( -0.2819296736111110424, 4.529944444520310753, -0.1167790944451423119 ) ) ;
#9058 = CARTESIAN_POINT ( 'NONE',  ( -0.4000000000000000222, 0.001785714090629508333, 0.1299678784931624920 ) ) ;
#9059 = CARTESIAN_POINT ( 'NONE',  ( 0.09528670647744390265, 4.518783353215682475, 0.2983507620828029783 ) ) ;
#9060 = CARTESIAN_POINT ( 'NONE',  ( -1.726321361862525858E-17, 5.130638888964754507, -0.2819296736111110979 ) ) ;
#9061 = DIRECTION ( 'NONE',  ( 0.8635502596144278842, 0.07555085810113110201, 0.4985709748471494618 ) ) ;
#9062 = DIRECTION ( 'NONE',  ( -0.000000000000000000, -1.000000000000000000, -0.000000000000000000 ) ) ;
#9063 = DIRECTION ( 'NONE',  ( 0.000000000000000000, 0.000000000000000000, -1.000000000000000000 ) ) ;
#9064 = FACE_OUTER_BOUND ( 'NONE', #19278, .T. ) ;
#9065 = CARTESIAN_POINT ( 'NONE',  ( 5.731347020009612645E-17, 4.238277777929510215, 0.3119999999999999996 ) ) ;
#9066 = CARTESIAN_POINT ( 'NONE',  ( 0.1993543840281266633, 4.568138888964755395, -0.1993543840281266910 ) ) ;
#9067 = CARTESIAN_POINT ( 'NONE',  ( -0.1993543840281266355, 3.748694444520309865, 0.1993543840281267465 ) ) ;
#9068 = ORIENTED_EDGE ( 'NONE', *, *, #17600, .T. ) ;
#9069 = ORIENTED_EDGE ( 'NONE', *, *, #12017, .F. ) ;
#9070 = ADVANCED_FACE ( 'NONE', ( #7780 ), #1927, .T. ) ;
#9071 = APPROVAL_ROLE ( '' ) ;
#9072 = CARTESIAN_POINT ( 'NONE',  ( -0.2552321839961925742, -0.1601952157747160432, 0.4125377734234058624 ) ) ;
#9073 = DIRECTION ( 'NONE',  ( 1.049727191138618079E-16, -0.5150380749100549327, 0.8571673007021117785 ) ) ;
#9074 = CARTESIAN_POINT ( 'NONE',  ( -0.5116234456863258950, 4.901168349308694161, -2.825533243875552269 ) ) ;
#9075 = ORIENTED_EDGE ( 'NONE', *, *, #20953, .F. ) ;
#9076 = CARTESIAN_POINT ( 'NONE',  ( 1.910449006669871087E-17, 0.1916666665149337478, -0.3119999999999999996 ) ) ;
#9077 = DIRECTION ( 'NONE',  ( 0.000000000000000000, 0.000000000000000000, -1.000000000000000000 ) ) ;
#9078 = CARTESIAN_POINT ( 'NONE',  ( -0.2779820761605299451, 5.119293720360404087, 0.1354021004295479780 ) ) ;
#9079 = CARTESIAN_POINT ( 'NONE',  ( -0.1292346314604056190, 0.2576388888888885287, -0.3119999999999999996 ) ) ;
#9080 = CARTESIAN_POINT ( 'NONE',  ( 1.573500000000000343, -3.414809992080329023E-17, -1.875000000000000000 ) ) ;
#9081 = VERTEX_POINT ( 'NONE', #2052 ) ;
#9082 = CARTESIAN_POINT ( 'NONE',  ( -0.2233192592356399442, 0.03660714275960045422, -0.3073725909049499494 ) ) ;
#9083 = CARTESIAN_POINT ( 'NONE',  ( 0.05068837741648516554, 5.073009555618063438, 0.3078549794868774558 ) ) ;
#9084 = CARTESIAN_POINT ( 'NONE',  ( 0.1954553509668046640, -0.1954553509668047195, 0.3313888888888926743 ) ) ;
#9085 = CONICAL_SURFACE ( 'NONE', #6753, 0.4062499999999995004, 0.7853981633974482790 ) ;
#9086 = CARTESIAN_POINT ( 'NONE',  ( -0.1993543840281266355, 4.304250000075865223, 0.1993543840281267465 ) ) ;
#9087 = CARTESIAN_POINT ( 'NONE',  ( -0.1167790944451423535, 5.141055555631421470, 0.2819296736111110979 ) ) ;
#9088 = CARTESIAN_POINT ( 'NONE',  ( 0.2887653152721417760, -0.08545421435188853276, 0.4122949633718255291 ) ) ;
#9089 = CARTESIAN_POINT ( 'NONE',  ( -0.2206810875299578256, 4.231324935242756879, 0.2214992208011696551 ) ) ;
#9090 = CARTESIAN_POINT ( 'NONE',  ( 0.3119999999999999996, 4.019527777777777366, 0.1292346314604056190 ) ) ;
#9091 = CARTESIAN_POINT ( 'NONE',  ( -0.2206173157302027676, 5.064666666818399499, 0.2206173157302028787 ) ) ;
#9092 = CARTESIAN_POINT ( 'NONE',  ( 4.589422455927707524E-07, 4.793851445074613693, 0.3119999999992840167 ) ) ;
#9093 = CARTESIAN_POINT ( 'NONE',  ( 0.1292346314604095325, 4.845916666666666650, 0.3119999999999962248 ) ) ;
#9094 = EDGE_LOOP ( 'NONE', ( #23525, #20294, #15294, #7290, #2147, #6156, #9798 ) ) ;
#9095 = APPROVAL ( #193, 'UNSPECIFIED' ) ;
#9096 = CARTESIAN_POINT ( 'NONE',  ( -0.1060100004866296602, 0.05877850679265330530, 0.2896447613046597702 ) ) ;
#9097 = ORIENTED_EDGE ( 'NONE', *, *, #17829, .F. ) ;
#9098 = VECTOR ( 'NONE', #19763, 39.37007874015748143 ) ;
#9099 = CARTESIAN_POINT ( 'NONE',  ( -0.1306872919485614903, 0.3155070326520293400, 0.1664583333333360671 ) ) ;
#9100 = CARTESIAN_POINT ( 'NONE',  ( -0.2819296736111110979, 5.075083333409198261, 0.000000000000000000 ) ) ;
#9101 = CARTESIAN_POINT ( 'NONE',  ( 0.08099032061186588194, -0.4945060939582642812, 0.4113389257669841648 ) ) ;
#9102 = CARTESIAN_POINT ( 'NONE',  ( 0.1116596296178199027, 0.4080357141881718608, 0.3436530038418508792 ) ) ;
#9103 = CARTESIAN_POINT ( 'NONE',  ( 0.2819296736111110979, 0.3305555554796889561, -0.1167790944451422980 ) ) ;
#9104 = CARTESIAN_POINT ( 'NONE',  ( -3.385114897866767815E-17, -0.2764156081756484196, 0.2202777777777806811 ) ) ;
#9105 = B_SPLINE_CURVE_WITH_KNOTS ( 'NONE', 3,
 ( #10390, #23275, #13922, #14152, #2580, #4876, #17812, #12223, #15747, #9901 ),
 .UNSPECIFIED., .F., .F.,
 ( 4, 2, 2, 2, 4 ),
 ( 1.355252715606880543E-19, 0.003321633220911224694, 0.006643266441822449388, 0.009964899662733674515, 0.01328653288364489878 ),
 .UNSPECIFIED. ) ;
#9106 = CARTESIAN_POINT ( 'NONE',  ( -0.1167790944451423535, 4.988277777853642903, 0.2819296736111110424 ) ) ;
#9107 = CARTESIAN_POINT ( 'NONE',  ( 0.05409597954341190812, 4.486773822218035335, -0.3072748769328391694 ) ) ;
#9108 = ORIENTED_EDGE ( 'NONE', *, *, #17048, .T. ) ;
#9109 = CARTESIAN_POINT ( 'NONE',  ( -0.2819296736111110424, 4.793833333409199149, -0.1167790944451423119 ) ) ;
#9110 = CARTESIAN_POINT ( 'NONE',  ( -0.2492977952293752575, 4.162941096864973822, -0.1919975030541300476 ) ) ;
#9111 = LINE ( 'NONE', #16561, #15214 ) ;
#9112 = CARTESIAN_POINT ( 'NONE',  ( -0.5116234456863466562, 3.514980167629567998, 2.722575290337332365 ) ) ;
#9113 = CARTESIAN_POINT ( 'NONE',  ( 1.967764614661186462, 2.340112590966282546, -1.877107582790499052 ) ) ;
#9114 = CARTESIAN_POINT ( 'NONE',  ( 0.3119999999999999996, 4.630638888888888971, 0.1292346314604056190 ) ) ;
#9115 = B_SPLINE_CURVE_WITH_KNOTS ( 'NONE', 3,
 ( #8652, #10500, #4992, #19632, #6707, #17571 ),
 .UNSPECIFIED., .F., .F.,
 ( 4, 2, 4 ),
 ( 0.006549771828772165717, 0.009815671976345301253, 0.01308157212391843766 ),
 .UNSPECIFIED. ) ;
#9116 = CARTESIAN_POINT ( 'NONE',  ( 0.1993543840281266633, 4.109805555631420582, -0.1993543840281266910 ) ) ;
#9117 = VECTOR ( 'NONE', #9851, 39.37007874015748143 ) ;
#9118 = CARTESIAN_POINT ( 'NONE',  ( -0.5116234456863258950, 5.163786281674128453, -3.093841259513817388 ) ) ;
#9119 = CARTESIAN_POINT ( 'NONE',  ( 0.2962862119097752212, 4.032746098098823673, -0.09776748290151990317 ) ) ;
#9120 = CARTESIAN_POINT ( 'NONE',  ( -0.01298396664829147909, 0.5473896884649155359, 0.04271845132552260643 ) ) ;
#9121 = ORIENTED_EDGE ( 'NONE', *, *, #18577, .T. ) ;
#9122 = DIRECTION ( 'NONE',  ( 0.000000000000000000, 0.000000000000000000, -1.000000000000000000 ) ) ;
#9123 = ORIENTED_EDGE ( 'NONE', *, *, #22229, .F. ) ;
#9124 = CARTESIAN_POINT ( 'NONE',  ( 0.2819296736111110424, 4.273000000075865223, -0.1167790944451423396 ) ) ;
#9125 = ADVANCED_FACE ( 'NONE', ( #18634 ), #17045, .T. ) ;
#9126 =( BOUNDED_CURVE ( )  B_SPLINE_CURVE ( 2, ( #17033, #13518, #2040, #565, #14974, #6171, #4226, #4102, #3871, #22396, #9723, #19102, #18866 ),
 .UNSPECIFIED., .F., .F. ) 
 B_SPLINE_CURVE_WITH_KNOTS ( ( 3, 2, 2, 2, 2, 2, 3 ),
 ( 0.8928571428571429047, 0.9000000000000000222, 0.9142857142857142572, 0.9285714285714286031, 0.9428571428571428381, 0.9571428571428571841, 0.9642857142857143016 ),
 .UNSPECIFIED. ) 
 CURVE ( )  GEOMETRIC_REPRESENTATION_ITEM ( )  RATIONAL_B_SPLINE_CURVE ( ( 0.9755282581475768211, 0.9755282581475769321, 1.000000000000000000, 0.9510565162951535312, 1.000000000000000000, 0.9510565162951535312, 1.000000000000000000, 0.9510565162951535312, 1.000000000000000000, 0.9510565162951535312, 1.000000000000000000, 0.9755282581475768211, 0.9755282581475768211 ) ) 
 REPRESENTATION_ITEM ( '' )  );
#9127 = AXIS2_PLACEMENT_3D ( 'NONE', #15878, #23181, #23294 ) ;
#9128 = CARTESIAN_POINT ( 'NONE',  ( -0.3118270672008495725, 4.114353485223650075, 0.03906138359714995262 ) ) ;
#9129 = CARTESIAN_POINT ( 'NONE',  ( 0.2206173157302028232, 0.08055555555555521385, -0.2206173157302028232 ) ) ;
#9130 = CARTESIAN_POINT ( 'NONE',  ( -3.385114897866767815E-17, -0.2764156081756484196, 0.3244444444444482545 ) ) ;
#9131 = AXIS2_PLACEMENT_3D ( 'NONE', #1158, #16038, #6761 ) ;
#9132 = CARTESIAN_POINT ( 'NONE',  ( 1.573500000000000343, 0.05625000000000004996, -1.412500000000000089 ) ) ;
#9133 = CARTESIAN_POINT ( 'NONE',  ( -0.3038752989638471846, 4.449004309992175443, 0.08168146717636678988 ) ) ;
#9134 = CARTESIAN_POINT ( 'NONE',  ( -8.251178249108312710E-07, 5.016022433328296337, 0.3119999999976432181 ) ) ;
#9135 = CARTESIAN_POINT ( 'NONE',  ( 0.2923287055106771337, 0.3758928570453146656, -0.2123892367102620249 ) ) ;
#9136 = CARTESIAN_POINT ( 'NONE',  ( 0.2819296736111110424, 0.1499999999241333482, -0.1167790944451423119 ) ) ;
#9137 = CARTESIAN_POINT ( 'NONE',  ( 0.4687500000000003331, -0.2150879084408183761, 0.05816236869046900737 ) ) ;
#9139 = CARTESIAN_POINT ( 'NONE',  ( 0.000000000000000000, 0.4199999999999998734, 0.2500000000000000555 ) ) ;
#9138 = B_SPLINE_CURVE_WITH_KNOTS ( 'NONE', 3,
 ( #10234, #13419, #19247, #21322, #4612, #17662, #948, #22905, #13773, #4255, #19019, #17304, #11706, #13666, #596, #10000, #17188, #8378, #474, #2669, #6080, #15715, #23129, #5958, #22669, #15479, #7906, #2314, #15358, #13547, #23372, #1318, #16198, #5203, #10836, #17781, #21681, #8743, #18144, #6804, #16315, #14245, #19971, #12312, #14364, #1199, #21439, #23488, #19844, #23612, #5083, #12677, #20094, #14125, #19725 ),
 .UNSPECIFIED., .F., .F.,
 ( 4, 2, 2, 1, 2, 2, 1, 1, 1, 2, 2, 2, 2, 2, 2, 2, 2, 2, 2, 1, 2, 2, 1, 1, 2, 2, 2, 2, 1, 1, 2, 4 ),
 ( 0.3932770965733057844, 0.3955159922397885608, 0.3957958541980989287, 0.3958133455704933024, 0.3958220912566904892, 0.3958308369428876761, 0.3958658196876764790, 0.3959357851772540293, 0.3960757161564091855, 0.3966354400730296992, 0.3977548879062707821, 0.3999937835727528923, 0.4011132314059939197, 0.4022326792392350026, 0.4033521270724760299, 0.4044715749057171128, 0.4055910227389581402, 0.4067104705721992230, 0.4072701944888197367, 0.4073401599783972871, 0.4073576513507917163, 0.4073751427231860900, 0.4074101254679748929, 0.4075500564471299936, 0.4078299184054402504, 0.4089493662386812778, 0.4100688140719223052, 0.4106285379885428188, 0.4109083999468530757, 0.4110483309260082319, 0.4111182964155857822, 0.4111882619051633325 ),
 .UNSPECIFIED. ) ;
#9140 = CARTESIAN_POINT ( 'NONE',  ( -0.1444244075563662910, 0.5295867991985312440, -0.7359786888858205200 ) ) ;
#9141 = CARTESIAN_POINT ( 'NONE',  ( -0.2764156081756484196, 0.1144950937579609918, -0.1304166666666665420 ) ) ;
#9142 = VERTEX_POINT ( 'NONE', #11447 ) ;
#9143 = ORIENTED_EDGE ( 'NONE', *, *, #19919, .T. ) ;
#9144 = CARTESIAN_POINT ( 'NONE',  ( -0.2045975126714155434, 5.098224757089310444, -0.2344162392893719138 ) ) ;
#9145 = MANIFOLD_SOLID_BREP ( 'Chamfer2 .050"', #20082 ) ;
#9146 = LINE ( 'NONE', #16590, #8976 ) ;
#9147 = VERTEX_POINT ( 'NONE', #4297 ) ;
#9148 = CARTESIAN_POINT ( 'NONE',  ( 0.3119999999999999996, -0.03750000000000033168, 0.000000000000000000 ) ) ;
#9149 = CARTESIAN_POINT ( 'NONE',  ( -0.1993543840281266910, 3.748694444520310309, -0.1993543840281266910 ) ) ;
#9150 = CARTESIAN_POINT ( 'NONE',  ( -6.979263641208234666E-17, 0.2080357141881718497, 0.3799334167787516425 ) ) ;
#9151 = CARTESIAN_POINT ( 'NONE',  ( 0.2819296736111110979, 4.338972222298087544, -3.452642723725051716E-17 ) ) ;
#9152 = CARTESIAN_POINT ( 'NONE',  ( 0.2206173157302028232, 0.1291666665149337201, -0.2206173157302028232 ) ) ;
#9153 = CARTESIAN_POINT ( 'NONE',  ( 0.3125000000000000000, -5.740531871003217465E-17, 0.3661111111111149397 ) ) ;
#9154 = ORIENTED_EDGE ( 'NONE', *, *, #22688, .F. ) ;
#9155 = CARTESIAN_POINT ( 'NONE',  ( 0.2597711826752152064, 4.358053561029723078, 0.1728091967789982530 ) ) ;
#9156 = CARTESIAN_POINT ( 'NONE',  ( -0.2819296736111110424, 4.911888888964754507, 0.1167790944451424923 ) ) ;
#9157 = EDGE_CURVE ( 'NONE', #20226, #19257, #9372, .T. ) ;
#9158 = CARTESIAN_POINT ( 'NONE',  ( 0.2947569499035622154, 4.199647669654026139, -0.1038884209671450953 ) ) ;
#9159 = LENGTH_MEASURE_WITH_UNIT ( LENGTH_MEASURE( 0.02539999999999999897 ), #21843 );
#9160 = CARTESIAN_POINT ( 'NONE',  ( 0.1236067977499789028, 0.1714285714285714024, 0.3804226065180614791 ) ) ;
#9161 = LOCAL_TIME ( 21, 9, 13.00000000000000000, #16638 ) ;
#9162 = CARTESIAN_POINT ( 'NONE',  ( -1.726321361862525858E-17, 4.561194444520309865, -0.2819296736111110979 ) ) ;
#9163 = COORDINATED_UNIVERSAL_TIME_OFFSET ( 0, 0, .AHEAD. ) ;
#9164 = FACE_OUTER_BOUND ( 'NONE', #22141, .T. ) ;
#9165 = CARTESIAN_POINT ( 'NONE',  ( 0.2206173157302027954, 4.918833333333332725, -0.2206173157302028232 ) ) ;
#9166 = CARTESIAN_POINT ( 'NONE',  ( 0.1993543840281266910, 0.5562499999241333759, -0.1993543840281266910 ) ) ;
#9167 = EDGE_LOOP ( 'NONE', ( #6635, #6759, #13212, #9639 ) ) ;
#9168 = ORIENTED_EDGE ( 'NONE', *, *, #1131, .F. ) ;
#9169 = CARTESIAN_POINT ( 'NONE',  ( 0.2819296736111110424, 0.1569444443685778234, 0.1167790944451424923 ) ) ;
#9170 = DIRECTION ( 'NONE',  ( -0.000000000000000000, 1.000000000000000000, -0.000000000000000000 ) ) ;
#9171 = CARTESIAN_POINT ( 'NONE',  ( -0.2659313529060423065, 5.198830554906272994, -0.1047787905467276182 ) ) ;
#9172 = CIRCLE ( 'NONE', #22799, 0.01875000000000000625 ) ;
#9173 = CARTESIAN_POINT ( 'NONE',  ( 2.575339694675500462E-17, 0.06071428571428567206, -0.4205848896953069405 ) ) ;
#9174 = CARTESIAN_POINT ( 'NONE',  ( 0.000000000000000000, 0.000000000000000000, 0.000000000000000000 ) ) ;
#9175 = CARTESIAN_POINT ( 'NONE',  ( -0.3096898932023051110, -0.3624663341596540134, 0.07654795713852843853 ) ) ;
#9176 = CARTESIAN_POINT ( 'NONE',  ( -0.001863919267159286786, 1.041821957232212270, -2.908070964936878333 ) ) ;
#9177 = CARTESIAN_POINT ( 'NONE',  ( 0.9396693423734434614, 2.384778440500604280, -1.315246104248910530 ) ) ;
#9178 = EDGE_CURVE ( 'NONE', #22290, #2118, #16925, .T. ) ;
#9179 = ADVANCED_FACE ( 'NONE', ( #9615 ), #578, .T. ) ;
#9180 = CARTESIAN_POINT ( 'NONE',  ( -0.2819296736111110424, 4.481333333409199149, 0.1167790944451424923 ) ) ;
#9181 = CARTESIAN_POINT ( 'NONE',  ( 0.3999999999999999667, 0.03035714266205807518, 0.1299678784931626307 ) ) ;
#9182 = CARTESIAN_POINT ( 'NONE',  ( 0.0005263094765449479037, 4.543818392271642637, -0.3119995841748594567 ) ) ;
#9183 = CARTESIAN_POINT ( 'NONE',  ( -0.1167790944451423257, 5.189666666742533074, -0.2819296736111110424 ) ) ;
#9184 = CARTESIAN_POINT ( 'NONE',  ( -0.1167790944451423119, 4.398000000075866112, -0.2819296736111110979 ) ) ;
#9185 = CARTESIAN_POINT ( 'NONE',  ( 0.2530760179677841171, 3.746625009379008109, 0.1847156476164619199 ) ) ;
#9186 = CC_DESIGN_APPROVAL ( #13608, ( #21185 ) ) ;
#9187 = LINE ( 'NONE', #16630, #21456 ) ;
#9188 = ORIENTED_EDGE ( 'NONE', *, *, #20646, .F. ) ;
#9189 = CARTESIAN_POINT ( 'NONE',  ( -0.4570242136016807177, 0.2774028246161669986, 0.04874733047933996893 ) ) ;
#9190 = CARTESIAN_POINT ( 'NONE',  ( -1.910449006669871087E-17, 4.043833333485065573, -0.3119999999999999996 ) ) ;
#9191 = EDGE_CURVE ( 'NONE', #5827, #6276, #16184, .T. ) ;
#9192 = CARTESIAN_POINT ( 'NONE',  ( -0.1993543840281266355, 4.595916666742532186, 0.1993543840281267465 ) ) ;
#9193 = CARTESIAN_POINT ( 'NONE',  ( -0.2819296736111110424, 3.849388888964754063, -0.1167790944451423119 ) ) ;
#9194 = VECTOR ( 'NONE', #11724, 39.37007874015748854 ) ;
#9195 = ORIENTED_EDGE ( 'NONE', *, *, #17515, .T. ) ;
#9196 = ORIENTED_EDGE ( 'NONE', *, *, #18763, .F. ) ;
#9197 = SHAPE_DEFINITION_REPRESENTATION ( #8951, #4350 ) ;
#9198 = CARTESIAN_POINT ( 'NONE',  ( -0.05458059743759432342, -0.3010824892324602819, 0.4171980187594044320 ) ) ;
#9199 = CARTESIAN_POINT ( 'NONE',  ( 5.731347020009612645E-17, 4.231333333333332725, 0.3119999999999999996 ) ) ;
#9200 = DIRECTION ( 'NONE',  ( 1.000000000000000000, 0.000000000000000000, 0.000000000000000000 ) ) ;
#9201 = CC_DESIGN_APPROVAL ( #10761, ( #1033 ) ) ;
#9202 = ORIENTED_EDGE ( 'NONE', *, *, #2472, .F. ) ;
#9203 = CARTESIAN_POINT ( 'NONE',  ( -0.2206173157302027954, 0.4208333331816004330, -0.2206173157302028232 ) ) ;
#9204 = CARTESIAN_POINT ( 'NONE',  ( -0.3124999999999993894, -0.1294417382415926909, 0.1820833333333360671 ) ) ;
#9205 = CARTESIAN_POINT ( 'NONE',  ( -0.03246180010856898612, 3.711382886895558286, -0.3109571910464125066 ) ) ;
#9206 = FACE_OUTER_BOUND ( 'NONE', #4312, .T. ) ;
#9207 = CARTESIAN_POINT ( 'NONE',  ( 5.463034709641816805E-17, 5.167344860100310910, 0.2973937581265823082 ) ) ;
#9208 = ORIENTED_EDGE ( 'NONE', *, *, #19371, .F. ) ;
#9209 = CARTESIAN_POINT ( 'NONE',  ( 0.1116596296178199860, 0.02589285704531474330, -0.3436530038418508792 ) ) ;
#9210 =( REPRESENTATION_RELATIONSHIP ('NONE','NONE', #4490, #7952 ) REPRESENTATION_RELATIONSHIP_WITH_TRANSFORMATION ( #7575 )SHAPE_REPRESENTATION_RELATIONSHIP( ) );
#9211 = AXIS2_PLACEMENT_3D ( 'NONE', #18462, #20535, #5534 ) ;
#9212 = ORIENTED_EDGE ( 'NONE', *, *, #6342, .F. ) ;
#9213 = LINE ( 'NONE', #21889, #2942 ) ;
#9214 = CARTESIAN_POINT ( 'NONE',  ( 0.1144950937579609085, -0.2764156081756484751, 0.3279166666666704089 ) ) ;
#9215 = CARTESIAN_POINT ( 'NONE',  ( -0.1167790944451423257, 4.231333333409199149, -0.2819296736111110424 ) ) ;
#9216 = CARTESIAN_POINT ( 'NONE',  ( 0.2819296736111111534, 5.154944444520309865, 0.1167790944451422563 ) ) ;
#9217 = CARTESIAN_POINT ( 'NONE',  ( -0.4687500000000002776, 0.08745190237456286486, 0.08858760123954044496 ) ) ;
#9218 = CARTESIAN_POINT ( 'NONE',  ( -0.3082045718900721654, 4.225735098311363735, 0.04853676656518685073 ) ) ;
#9219 = CARTESIAN_POINT ( 'NONE',  ( 0.3119999999999999996, 3.915361111111111292, -0.1292346314604056745 ) ) ;
#9220 = EDGE_CURVE ( 'NONE', #9147, #14303, #931, .T. ) ;
#9221 = CARTESIAN_POINT ( 'NONE',  ( -0.3119999999999999996, 4.887583333485065573, -0.1292346314604056468 ) ) ;
#9222 = CARTESIAN_POINT ( 'NONE',  ( 0.3108175396127563217, 4.806979697495309622, 0.02714641660050034003 ) ) ;
#9223 = FACE_OUTER_BOUND ( 'NONE', #16796, .T. ) ;
#9224 = EDGE_LOOP ( 'NONE', ( #16031, #13979, #12073, #18882, #19458, #4430 ) ) ;
#9225 = PLANE ( 'NONE',  #17387 ) ;
#9226 = B_SPLINE_CURVE_WITH_KNOTS ( 'NONE', 3,
 ( #19593, #21430, #1065, #8494, #21546, #12303, #15820, #14117, #14234, #4717, #8623, #21671, #12423, #19836, #19477, #23360, #15936, #4835 ),
 .UNSPECIFIED., .F., .F.,
 ( 4, 2, 2, 2, 2, 2, 2, 2, 4 ),
 ( 0.9228889348174078577, 0.9251733130190006316, 0.9274576912205934054, 0.9297420694221861792, 0.9320264476237789530, 0.9343108258253717269, 0.9365952040269645007, 0.9388795822285572745, 0.9411639604301500484 ),
 .UNSPECIFIED. ) ;
#9227 = CARTESIAN_POINT ( 'NONE',  ( 0.05682895016479121153, 0.04205235519552708023, -0.2861892567955108269 ) ) ;
#9228 = VECTOR ( 'NONE', #261, 39.37007874015748854 ) ;
#9229 = CARTESIAN_POINT ( 'NONE',  ( -0.1306872919485615459, -0.3155070326520293400, 0.2428472222222255728 ) ) ;
#9230 = CARTESIAN_POINT ( 'NONE',  ( 0.1167790944451424368, 5.203555555631421470, 0.2819296736111110424 ) ) ;
#9231 = LINE ( 'NONE', #18616, #7983 ) ;
#9232 = CYLINDRICAL_SURFACE ( 'NONE', #5962, 0.2109499999999996656 ) ;
#9233 = CARTESIAN_POINT ( 'NONE',  ( 1.726321361862525858E-17, 0.2298611110352444531, -0.2819296736111110979 ) ) ;
#9234 = CARTESIAN_POINT ( 'NONE',  ( 0.1954553509668046640, -0.1954553509668047195, 0.2272222222222252119 ) ) ;
#9235 = CARTESIAN_POINT ( 'NONE',  ( 0.1993543840281267465, 4.887583333409199149, 0.1993543840281266633 ) ) ;
#9236 = DIRECTION ( 'NONE',  ( 1.000000000000000000, 0.000000000000000000, 0.000000000000000000 ) ) ;
#9237 = EDGE_LOOP ( 'NONE', ( #13429, #14363, #4168, #23596 ) ) ;
#9238 = CARTESIAN_POINT ( 'NONE',  ( 0.2819296736111110979, 4.825083333409199149, -3.452642723725051716E-17 ) ) ;
#9239 = CARTESIAN_POINT ( 'NONE',  ( -2.307748244742446386E-07, 4.182713274783838919, 0.3119999999998222528 ) ) ;
#9240 = CARTESIAN_POINT ( 'NONE',  ( -0.1292346314604057300, 5.061194444444443441, 0.3119999999999998885 ) ) ;
#9241 = CARTESIAN_POINT ( 'NONE',  ( -1.172879095217528311, 4.111524471938507119, -2.231985037876813127 ) ) ;
#9242 = CARTESIAN_POINT ( 'NONE',  ( 0.1720490635147988168, 0.06249999999999968081, 0.2634598316069546309 ) ) ;
#9243 = CARTESIAN_POINT ( 'NONE',  ( 5.731347020009612645E-17, 4.397999999999999687, 0.3119999999999999996 ) ) ;
#9244 = VECTOR ( 'NONE', #19189, 39.37007874015748143 ) ;
#9245 = CARTESIAN_POINT ( 'NONE',  ( 5.178964085587577574E-17, 3.977861111186976384, 0.2819296736111110979 ) ) ;
#9246 = CARTESIAN_POINT ( 'NONE',  ( -0.2819296736111110424, 3.863277777853644235, -0.1167790944451423119 ) ) ;
#9247 = CARTESIAN_POINT ( 'NONE',  ( 0.2963184418439536727, 4.032743120851792540, -0.09767001781238864033 ) ) ;
#9248 = CARTESIAN_POINT ( 'NONE',  ( 0.1292346314604031765, 4.422305555555555046, -0.3120000000000024420 ) ) ;
#9249 = EDGE_LOOP ( 'NONE', ( #14452, #13759, #17510, #23704, #21354 ) ) ;
#9250 = CARTESIAN_POINT ( 'NONE',  ( -0.006672437742759285313, -0.5374135436383427056, 0.05975564523638848130 ) ) ;
#9251 = CARTESIAN_POINT ( 'NONE',  ( -0.1733170103021690056, 4.121925038073740666, 0.2594324947820166316 ) ) ;
#9252 = CARTESIAN_POINT ( 'NONE',  ( 0.1684295338161674871, 4.632258567753597234, 0.2661145548031557673 ) ) ;
#9253 = CARTESIAN_POINT ( 'NONE',  ( 0.2764156081756484196, -5.077672346800151106E-17, 0.2272222222222252119 ) ) ;
#9254 = AXIS2_PLACEMENT_3D ( 'NONE', #10242, #6934, #10126 ) ;
#9255 = LINE ( 'NONE', #7544, #9556 ) ;
#9256 = DIRECTION ( 'NONE',  ( 0.000000000000000000, 1.000000000000000000, 0.000000000000000000 ) ) ;
#9257 = CARTESIAN_POINT ( 'NONE',  ( 1.573500000000000343, 2.740000000000000213, -1.874999999999999334 ) ) ;
#9258 = CARTESIAN_POINT ( 'NONE',  ( 0.3613381517857143232, 0.2294642856167432576, -0.1174058825155740587 ) ) ;
#9259 = CARTESIAN_POINT ( 'NONE',  ( -0.1993543840281267465, 0.2923611110352445364, 0.1993543840281266633 ) ) ;
#9260 = CARTESIAN_POINT ( 'NONE',  ( 0.3125000000000000000, -5.740531871003217465E-17, 0.1508333333333358728 ) ) ;
#9261 = CARTESIAN_POINT ( 'NONE',  ( 1.910449006669871087E-17, 0.5874999999999996891, -0.3119999999999999996 ) ) ;
#9262 = CC_DESIGN_PERSON_AND_ORGANIZATION_ASSIGNMENT ( #16370, #24027, ( #11937 ) ) ;
#9263 = DIRECTION ( 'NONE',  ( -0.000000000000000000, -1.000000000000000000, -0.000000000000000000 ) ) ;
#9264 = CARTESIAN_POINT ( 'NONE',  ( 0.2764156081756483641, -0.1144950937579611167, -0.1026388888888885437 ) ) ;
#9265 = ORIENTED_EDGE ( 'NONE', *, *, #10204, .F. ) ;
#9266 = ORIENTED_EDGE ( 'NONE', *, *, #13222, .F. ) ;
#9267 = DIRECTION ( 'NONE',  ( -0.8651979924482665618, 0.04370253788966840108, -0.4995222938423183878 ) ) ;
#9268 = CARTESIAN_POINT ( 'NONE',  ( 0.4687500000000002776, -0.2178881689638759445, 0.3900517602158629638 ) ) ;
#9269 = CARTESIAN_POINT ( 'NONE',  ( -0.2206173157302028787, 0.05277777777777744456, 0.2206173157302027954 ) ) ;
#9270 = CARTESIAN_POINT ( 'NONE',  ( 0.2819296736111110424, 3.842444444520310309, -0.1167790944451423396 ) ) ;
#9271 = CARTESIAN_POINT ( 'NONE',  ( -0.2923287055106771337, 0.1830357141881718552, -0.2123892367102620804 ) ) ;
#9272 = CARTESIAN_POINT ( 'NONE',  ( -0.2819296736111110424, 4.425777777853643791, 0.1167790944451424923 ) ) ;
#9273 = DIRECTION ( 'NONE',  ( 0.000000000000000000, 0.000000000000000000, -1.000000000000000000 ) ) ;
#9274 = CARTESIAN_POINT ( 'NONE',  ( -0.2206173157302028787, 0.1569444442927115102, 0.2206173157302027954 ) ) ;
#9275 = ORIENTED_EDGE ( 'NONE', *, *, #21097, .T. ) ;
#9276 = VECTOR ( 'NONE', #5047, 39.37007874015748143 ) ;
#9277 = CARTESIAN_POINT ( 'NONE',  ( 0.08374467998906506838, 4.374797057175100257, -0.3008178344637207902 ) ) ;
#9278 = CARTESIAN_POINT ( 'NONE',  ( -0.1167790944451423257, 4.842444444520309865, -0.2819296736111110424 ) ) ;
#9279 = CARTESIAN_POINT ( 'NONE',  ( 0.2209708691207961651, 0.2209708691207959985, -0.008888888888887605186 ) ) ;
#9280 = DIRECTION ( 'NONE',  ( -7.888609052210118054E-31, 1.000000000000000000, 1.577721810442023611E-30 ) ) ;
#9281 = CARTESIAN_POINT ( 'NONE',  ( -1.910449006669871087E-17, 4.981333333333332725, -0.3119999999999999996 ) ) ;
#9282 = CARTESIAN_POINT ( 'NONE',  ( 0.2819296736111111534, 4.710500000075865223, 0.1167790944451422563 ) ) ;
#9283 = APPROVAL_DATE_TIME ( #12846, #19391 ) ;
#9284 = CYLINDRICAL_SURFACE ( 'NONE', #9699, 0.3119999999999999996 ) ;
#9285 = CARTESIAN_POINT ( 'NONE',  ( -0.2819296736111110424, 0.5736111110352444253, -0.1167790944451423396 ) ) ;
#9287 = ORIENTED_EDGE ( 'NONE', *, *, #23604, .T. ) ;
#9286 = AXIS2_PLACEMENT_3D ( 'NONE', #22958, #6383, #6260 ) ;
#9288 = EDGE_LOOP ( 'NONE', ( #17733, #22023, #13389, #14532 ) ) ;
#9289 = CARTESIAN_POINT ( 'NONE',  ( -0.2819296736111110424, 0.2958333332574666907, -0.1167790944451423396 ) ) ;
#9290 = CARTESIAN_POINT ( 'NONE',  ( -1.054647954922321762E-07, 4.988277780858759947, -0.3119999999999820695 ) ) ;
#9291 = CARTESIAN_POINT ( 'NONE',  ( 0.7919466436700954848, 0.05000000000000028727, -2.986000000000000210 ) ) ;
#9292 = CARTESIAN_POINT ( 'NONE',  ( -0.2472135954999579999, 0.2321428571428570675, 0.3402603233408159622 ) ) ;
#9293 = CARTESIAN_POINT ( 'NONE',  ( -0.1306872919485615459, -0.3155070326520293400, 0.01715277777777886661 ) ) ;
#9294 = EDGE_CURVE ( 'NONE', #16753, #15714, #8960, .T. ) ;
#9295 = CARTESIAN_POINT ( 'NONE',  ( 0.000000000000000000, 5.500232050807569273, -0.2510000000000000009 ) ) ;
#9296 = CARTESIAN_POINT ( 'NONE',  ( -0.1696533514972167755, 3.882199842881781660, -0.2624525851558037748 ) ) ;
#9297 = CARTESIAN_POINT ( 'NONE',  ( -5.178964085587577574E-17, 0.2437499999241333204, 0.2819296736111110979 ) ) ;
#9298 = CARTESIAN_POINT ( 'NONE',  ( 0.9765096322779955873, 2.453214835500605595, -1.257424259103740116 ) ) ;
#9299 = CARTESIAN_POINT ( 'NONE',  ( 0.2819296736111110979, 4.616750000075865223, -3.452642723725051716E-17 ) ) ;
#9300 = CARTESIAN_POINT ( 'NONE',  ( -0.4000000000000000222, -0.001785714480799064936, -4.898587196589413075E-17 ) ) ;
#9301 = DIRECTION ( 'NONE',  ( 0.5773502691896256200, 0.5773502691896257311, -0.5773502691896257311 ) ) ;
#9302 = CARTESIAN_POINT ( 'NONE',  ( 0.2819296736111110979, 5.002166666742532186, 0.1167790944451422425 ) ) ;
#9303 = CARTESIAN_POINT ( 'NONE',  ( -0.1993543840281266355, 4.415361111186976828, 0.1993543840281267465 ) ) ;
#9304 = CARTESIAN_POINT ( 'NONE',  ( 0.06953549797911996733, 3.740285477686101867, 0.3047298766157227612 ) ) ;
#9305 = DIRECTION ( 'NONE',  ( 0.000000000000000000, 0.000000000000000000, -1.000000000000000000 ) ) ;
#9306 = DIRECTION ( 'NONE',  ( -0.000000000000000000, 1.000000000000000000, -0.000000000000000000 ) ) ;
#9307 = CARTESIAN_POINT ( 'NONE',  ( 0.3119999999999999996, 3.970916666818399055, 0.1292346314604056190 ) ) ;
#9308 = CARTESIAN_POINT ( 'NONE',  ( 0.1993543840281266633, 4.457027777853643791, -0.1993543840281266910 ) ) ;
#9309 = CARTESIAN_POINT ( 'NONE',  ( 0.3119999999999999996, 0.1291666666666663188, 0.000000000000000000 ) ) ;
#9310 = VECTOR ( 'NONE', #18379, 39.37007874015748143 ) ;
#9311 = CARTESIAN_POINT ( 'NONE',  ( -0.4116234456863466229, 1.808198851485060210, 2.607105236499406953 ) ) ;
#9312 = ORIENTED_EDGE ( 'NONE', *, *, #8092, .T. ) ;
#9313 = EDGE_CURVE ( 'NONE', #11401, #1686, #15196, .T. ) ;
#9314 = ADVANCED_FACE ( 'NONE', ( #16059 ), #23732, .T. ) ;
#9315 = ORIENTED_EDGE ( 'NONE', *, *, #14190, .T. ) ;
#9316 = COORDINATED_UNIVERSAL_TIME_OFFSET ( 0, 0, .AHEAD. ) ;
#9317 = CARTESIAN_POINT ( 'NONE',  ( -0.2977072594216396695, 1.822931211668208286E-17, 0.4093739260883065278 ) ) ;
#9318 = CARTESIAN_POINT ( 'NONE',  ( -0.1099907963434661878, 4.846209151129420079, 0.2920362175865332532 ) ) ;
#9319 = SPHERICAL_SURFACE ( 'NONE', #15903, 0.3119999999999999996 ) ;
#9320 = ORIENTED_EDGE ( 'NONE', *, *, #18851, .F. ) ;
#9321 = CARTESIAN_POINT ( 'NONE',  ( -0.1292346314604056190, 0.5840277776260447418, -0.3119999999999999996 ) ) ;
#9322 = ORIENTED_EDGE ( 'NONE', *, *, #11219, .F. ) ;
#9323 = CARTESIAN_POINT ( 'NONE',  ( -0.02441201398334205686, 3.066692553488282957, 3.451468604327566858 ) ) ;
#9324 = CARTESIAN_POINT ( 'NONE',  ( -0.09421363705610538708, 3.713154806801743923, -0.2985087040289488014 ) ) ;
#9325 = DIRECTION ( 'NONE',  ( -0.000000000000000000, -1.000000000000000000, -0.000000000000000000 ) ) ;
#9326 = CARTESIAN_POINT ( 'NONE',  ( -0.1292346314604058410, 0.5006944444444441089, 0.3119999999999998885 ) ) ;
#9327 = EDGE_CURVE ( 'NONE', #3971, #10527, #3891, .T. ) ;
#9328 = ORIENTED_EDGE ( 'NONE', *, *, #14352, .T. ) ;
#9329 = CARTESIAN_POINT ( 'NONE',  ( 2.326421213736078119E-17, 0.1723214284738861790, -0.3799334167787516980 ) ) ;
#9330 = VECTOR ( 'NONE', #10968, 39.37007874015748143 ) ;
#9331 = ORIENTED_EDGE ( 'NONE', *, *, #7090, .F. ) ;
#9332 = CARTESIAN_POINT ( 'NONE',  ( 0.4687500000000002776, -0.2706329386826372141, 0.4425000000000000044 ) ) ;
#9333 = CARTESIAN_POINT ( 'NONE',  ( -0.1144950937579609779, 0.2764156081756484196, 0.1890277777777805146 ) ) ;
#9334 = B_SPLINE_CURVE_WITH_KNOTS ( 'NONE', 3,
 ( #5281, #2976, #12749, #1510, #3331, #1269, #1023, #7122, #4794, #21629, #21987, #12624, #14075, #5036 ),
 .UNSPECIFIED., .F., .F.,
 ( 4, 2, 2, 2, 2, 2, 4 ),
 ( 0.002465611774710352224, 0.003521823575328993962, 0.004578035375947636133, 0.006690458977184919609, 0.007746670777803561780, 0.008802882578422202217, 0.01091530617965948656 ),
 .UNSPECIFIED. ) ;
#9335 = CARTESIAN_POINT ( 'NONE',  ( -0.2819296736111110424, 4.293833333409199149, -0.1167790944451423119 ) ) ;
#9336 = CARTESIAN_POINT ( 'NONE',  ( 0.1167790944451424506, 5.036888888964754507, 0.2819296736111110424 ) ) ;
#9337 = CARTESIAN_POINT ( 'NONE',  ( -0.1366666852802201904, -0.4623613298295002894, 0.4215068951509234885 ) ) ;
#9338 = DIRECTION ( 'NONE',  ( 1.224646799147352468E-16, 0.000000000000000000, -1.000000000000000000 ) ) ;
#9339 = CARTESIAN_POINT ( 'NONE',  ( 0.1292346314604056190, 3.922305555555555046, -0.3119999999999999996 ) ) ;
#9340 = CARTESIAN_POINT ( 'NONE',  ( -0.2206173157302027676, 4.842444444596176290, 0.2206173157302028787 ) ) ;
#9341 = CARTESIAN_POINT ( 'NONE',  ( 0.2852864521860641323, 4.804037699710621112, 0.1277937968658160450 ) ) ;
#9342 = CARTESIAN_POINT ( 'NONE',  ( 0.1292346314604057300, 0.3965277777777774237, 0.3119999999999998885 ) ) ;
#9343 = CARTESIAN_POINT ( 'NONE',  ( -0.1116596296178199582, 0.08660714275960045005, -0.3436530038418508792 ) ) ;
#9344 =( BOUNDED_CURVE ( )  B_SPLINE_CURVE ( 2, ( #13201, #22441, #11356, #16954, #18784, #11601, #9279, #19032, #7811 ),
 .UNSPECIFIED., .F., .F. ) 
 B_SPLINE_CURVE_WITH_KNOTS ( ( 3, 2, 2, 2, 3 ),
 ( 0.6562500000000001110, 0.6666666666666668517, 0.6770833333333334814, 0.6875000000000000000, 0.6979166666666667407 ),
 .UNSPECIFIED. ) 
 CURVE ( )  GEOMETRIC_REPRESENTATION_ITEM ( )  RATIONAL_B_SPLINE_CURVE ( ( 0.9999999999999992228, 0.9238795325112875156, 1.000000000000000000, 0.9238795325112867385, 1.000000000000000000, 0.9238795325112867385, 1.000000000000000000, 0.9238795325112867385, 1.000000000000000000 ) ) 
 REPRESENTATION_ITEM ( '' )  );
#9345 = VECTOR ( 'NONE', #7846, 39.37007874015748143 ) ;
#9346 = CARTESIAN_POINT ( 'NONE',  ( 0.2838164519978598754, 0.03466679542269811981, -0.01821027516514309857 ) ) ;
#9347 = AXIS2_PLACEMENT_3D ( 'NONE', #3764, #2417, #6064 ) ;
#9348 = ORIENTED_EDGE ( 'NONE', *, *, #20795, .F. ) ;
#9349 = COORDINATED_UNIVERSAL_TIME_OFFSET ( 0, 0, .AHEAD. ) ;
#9350 = CARTESIAN_POINT ( 'NONE',  ( -0.2819296736111110424, 5.189666666742532186, 0.1167790944451424923 ) ) ;
#9351 =( REPRESENTATION_RELATIONSHIP ('NONE','NONE', #4490, #12001 ) REPRESENTATION_RELATIONSHIP_WITH_TRANSFORMATION ( #2801 )SHAPE_REPRESENTATION_RELATIONSHIP( ) );
#9352 = CARTESIAN_POINT ( 'NONE',  ( 0.04612934949352820446, -0.5146330850176437099, 0.3902021065396754085 ) ) ;
#9353 = PRODUCT_DEFINITION_SHAPE ( 'NONE', 'NONE',  #24135 ) ;
#9354 = DIRECTION ( 'NONE',  ( 0.8660254037844433705, 0.000000000000000000, 0.4999999999999916178 ) ) ;
#9355 = VERTEX_POINT ( 'NONE', #21306 ) ;
#9356 = CARTESIAN_POINT ( 'NONE',  ( 0.1993543840281266910, 0.2229166665908000333, -0.1993543840281266910 ) ) ;
#9357 = CARTESIAN_POINT ( 'NONE',  ( -0.2764156081756484196, -0.1144950937579609362, 0.2654166666666699093 ) ) ;
#9358 = CARTESIAN_POINT ( 'NONE',  ( 0.1167790944451424368, 5.050777777853643791, 0.2819296736111110424 ) ) ;
#9359 = CARTESIAN_POINT ( 'NONE',  ( 0.05463760851107932887, 4.486759113827675449, -0.3071788916223130439 ) ) ;
#9360 = CARTESIAN_POINT ( 'NONE',  ( 0.1167790944451424368, 4.925777777853642903, 0.2819296736111110424 ) ) ;
#9361 = CARTESIAN_POINT ( 'NONE',  ( -0.2472135954999579999, 0.08035714266205803979, 0.3402603233408160732 ) ) ;
#9362 = AXIS2_PLACEMENT_3D ( 'NONE', #1047, #15915, #4940 ) ;
#9363 = DIRECTION ( 'NONE',  ( -1.000000000000000000, 0.000000000000000000, 0.000000000000000000 ) ) ;
#9364 = CARTESIAN_POINT ( 'NONE',  ( 5.731347020009612645E-17, 4.897999999999998799, 0.3119999999999999996 ) ) ;
#9365 = DIRECTION ( 'NONE',  ( 0.000000000000000000, 0.000000000000000000, -1.000000000000000000 ) ) ;
#9366 = CARTESIAN_POINT ( 'NONE',  ( 0.3119999999999999996, 4.470916666666665762, -0.1292346314604056745 ) ) ;
#9367 = CONICAL_SURFACE ( 'NONE', #18708, 0.4453125000000000000, 1.047197551196600074 ) ;
#9368 = CARTESIAN_POINT ( 'NONE',  ( -0.1993543840281266910, 3.845916666742532186, -0.1993543840281266910 ) ) ;
#9369 = DIRECTION ( 'NONE',  ( -0.7071067811865475727, -0.7071067811865475727, -0.000000000000000000 ) ) ;
#9370 = CARTESIAN_POINT ( 'NONE',  ( 0.1923084850919542510, 4.021960649823486555, 0.2457072462168881366 ) ) ;
#9371 = PLANE ( 'NONE',  #11331 ) ;
#9372 = LINE ( 'NONE', #15342, #17502 ) ;
#9373 = ORIENTED_EDGE ( 'NONE', *, *, #21094, .F. ) ;
#9374 = CARTESIAN_POINT ( 'NONE',  ( -0.2935801054093536977, 4.116470801662853951, 0.1121277540818491902 ) ) ;
#9375 = CARTESIAN_POINT ( 'NONE',  ( -3.990790521751304672E-07, 4.654944455680286808, -0.3119999999997447038 ) ) ;
#9376 = AXIS2_PLACEMENT_3D ( 'NONE', #9572, #22852, #7738 ) ;
#9377 = CARTESIAN_POINT ( 'NONE',  ( 0.1954553509668047195, 0.1954553509668046085, 0.2897222222222257115 ) ) ;
#9378 = AXIS2_PLACEMENT_3D ( 'NONE', #22794, #23924, #19136 ) ;
#9379 = ADVANCED_FACE ( 'NONE', ( #4474 ), #2879, .T. ) ;
#9380 = CARTESIAN_POINT ( 'NONE',  ( 1.471352214327352081, 2.291712385858714285, -1.221931094509318694 ) ) ;
#9381 = CARTESIAN_POINT ( 'NONE',  ( 0.4739766090219372785, 0.2774257203002796213, 0.04193793378272820532 ) ) ;
#9382 = EDGE_CURVE ( 'NONE', #18897, #8797, #10966, .T. ) ;
#9383 = ORIENTED_EDGE ( 'NONE', *, *, #8117, .F. ) ;
#9384 = CARTESIAN_POINT ( 'NONE',  ( -0.2923287055106771337, 0.3258928570453146767, -0.2123892367102620804 ) ) ;
#9385 = CARTESIAN_POINT ( 'NONE',  ( -0.2819296736111110979, 0.2888888888130223265, 0.1167790944451422425 ) ) ;
#9386 = CARTESIAN_POINT ( 'NONE',  ( 0.2726250823473003182, 3.867817045068989934, -0.1571225677078837979 ) ) ;
#9387 = CARTESIAN_POINT ( 'NONE',  ( 0.1113574050366882423, 0.7676397398856372734, -1.079857189324826550 ) ) ;
#9388 = CARTESIAN_POINT ( 'NONE',  ( -0.2206173157302027954, 0.1499999999999996336, -0.2206173157302028232 ) ) ;
#9389 = CARTESIAN_POINT ( 'NONE',  ( 0.000000000000000000, 0.2764156081756484196, 0.02583333333333468970 ) ) ;
#9390 = CARTESIAN_POINT ( 'NONE',  ( -0.09984127256979968834, 5.094866437056988495, -0.2954929550594492249 ) ) ;
#9391 = CARTESIAN_POINT ( 'NONE',  ( 0.4687500000000002776, -0.08748112355138647211, 0.4143798302908627273 ) ) ;
#9392 = CARTESIAN_POINT ( 'NONE',  ( 1.910449006669871087E-17, 0.08749999999999966138, -0.3119999999999999996 ) ) ;
#9393 = CARTESIAN_POINT ( 'NONE',  ( 0.1292346314604056190, 5.200083333333331836, -0.3119999999999999996 ) ) ;
#9394 = CARTESIAN_POINT ( 'NONE',  ( 0.2233192592356399164, 0.1437499999024575981, 0.3073725909049500604 ) ) ;
#9395 = CARTESIAN_POINT ( 'NONE',  ( 0.2819296736111110979, 4.172305555631421470, -3.452642723725051716E-17 ) ) ;
#9396 = DIRECTION ( 'NONE',  ( -0.8660254037844434816, 0.000000000000000000, 0.4999999999999913403 ) ) ;
#9397 = CARTESIAN_POINT ( 'NONE',  ( 0.4000000000000000222, 0.3910714283763437327, 0.000000000000000000 ) ) ;
#9398 = ORIENTED_EDGE ( 'NONE', *, *, #23780, .F. ) ;
#9399 = ORIENTED_EDGE ( 'NONE', *, *, #18211, .F. ) ;
#9400 = CARTESIAN_POINT ( 'NONE',  ( 0.1569501933412678629, 4.353958851224170701, 0.2727168492022662427 ) ) ;
#9401 = CARTESIAN_POINT ( 'NONE',  ( 0.2819296736111110979, 4.936194444520309865, -3.452642723725051716E-17 ) ) ;
#9402 = CARTESIAN_POINT ( 'NONE',  ( -0.2740592345421557496, 5.152155295800852741, -0.1267607899272875649 ) ) ;
#9403 = CARTESIAN_POINT ( 'NONE',  ( 0.1711834221389471333, 3.705440968472438534, -0.2633095395294266505 ) ) ;
#9404 = CC_DESIGN_PERSON_AND_ORGANIZATION_ASSIGNMENT ( #4626, #23266, ( #22007 ) ) ;
#9405 = CARTESIAN_POINT ( 'NONE',  ( -0.2206173157302027676, 5.002166666666665762, 0.2206173157302028787 ) ) ;
#9406 = CARTESIAN_POINT ( 'NONE',  ( 5.178964085587577574E-17, 4.644527777853642903, 0.2819296736111110979 ) ) ;
#9407 = PERSON_AND_ORGANIZATION_ROLE ( 'classification_officer' ) ;
#9408 = CARTESIAN_POINT ( 'NONE',  ( 1.171015175950385068, 4.111524471938507119, -0.8765847808846783940 ) ) ;
#9409 = DIRECTION ( 'NONE',  ( 0.000000000000000000, 0.000000000000000000, 1.000000000000000000 ) ) ;
#9410 = CARTESIAN_POINT ( 'NONE',  ( 0.2819296736111110424, 0.4972222221463556413, -0.1167790944451423119 ) ) ;
#9411 = EDGE_LOOP ( 'NONE', ( #9154, #17982, #3854, #19272 ) ) ;
#9412 = EDGE_LOOP ( 'NONE', ( #3110, #8076, #20645, #15644 ) ) ;
#9413 = CARTESIAN_POINT ( 'NONE',  ( -0.1167790944451424368, 0.3097222221463556968, 0.2819296736111110424 ) ) ;
#9414 = CARTESIAN_POINT ( 'NONE',  ( -0.1241992254576447796, 4.714064213952139148, -0.2879476753977870396 ) ) ;
#9415 = CARTESIAN_POINT ( 'NONE',  ( -0.4000000000000000222, 0.3553571426620580342, -4.898587196589413075E-17 ) ) ;
#9416 = CARTESIAN_POINT ( 'NONE',  ( 0.1236067977499789028, 0.3142857142857142239, 0.3804226065180614791 ) ) ;
#9417 = CARTESIAN_POINT ( 'NONE',  ( 0.1306872919485616846, 0.3155070326520292290, 0.04493055555555688918 ) ) ;
#9418 = CARTESIAN_POINT ( 'NONE',  ( -0.2209708691207961373, -0.2209708691207961095, 0.01888888888889038095 ) ) ;
#9419 = DIRECTION ( 'NONE',  ( -0.000000000000000000, 0.2588190451025213501, -0.9659258262890682012 ) ) ;
#9420 = CARTESIAN_POINT ( 'NONE',  ( 0.1167790944451423535, 0.3583333332574666907, 0.2819296736111110979 ) ) ;
#9421 = CARTESIAN_POINT ( 'NONE',  ( 1.101325272654156251, 2.384774948516263482, -1.035249514148854466 ) ) ;
#9422 = CARTESIAN_POINT ( 'NONE',  ( -0.1167790944451423257, 4.189666666742533074, -0.2819296736111110424 ) ) ;
#9423 = CARTESIAN_POINT ( 'NONE',  ( -0.4000000000000000222, 0.1446428569477723469, 0.1299678784931624920 ) ) ;
#9424 = CARTESIAN_POINT ( 'NONE',  ( 0.1993543840281266633, 4.845916666742532186, -0.1993543840281266910 ) ) ;
#9425 = CARTESIAN_POINT ( 'NONE',  ( 0.1993543840281266633, 4.498694444520309865, -0.1993543840281266910 ) ) ;
#9426 = DIRECTION ( 'NONE',  ( -0.000000000000000000, -1.000000000000000000, -0.000000000000000000 ) ) ;
#9427 = ORIENTED_EDGE ( 'NONE', *, *, #8468, .T. ) ;
#9428 = CARTESIAN_POINT ( 'NONE',  ( 0.2195291445273800934, 3.925916276105013480, -0.2262840060551973564 ) ) ;
#9429 = ADVANCED_FACE ( 'NONE', ( #23233 ), #6542, .F. ) ;
#9430 = CARTESIAN_POINT ( 'NONE',  ( 5.731347020009612645E-17, 4.127166666818398610, 0.3119999999999999996 ) ) ;
#9431 = CARTESIAN_POINT ( 'NONE',  ( -0.3854970698558352060, 0.3186990403121960358, 0.4003306813560890132 ) ) ;
#9432 = EDGE_CURVE ( 'NONE', #20425, #22988, #12296, .T. ) ;
#9433 =( CONVERSION_BASED_UNIT ( 'INCH', #1995 ) LENGTH_UNIT ( ) NAMED_UNIT ( #17887 ) );
#9434 = EDGE_LOOP ( 'NONE', ( #20916, #6631, #2576, #20601, #5508, #14178, #19603, #11664, #13002, #887, #12809, #15041, #19231, #16530, #22076, #7984, #23428, #12034, #22066, #17277, #9568, #24086, #14019, #11839, #19303, #7878 ) ) ;
#9435 = EDGE_LOOP ( 'NONE', ( #22192, #3142, #21781, #16637, #8370, #9706, #18612 ) ) ;
#9436 = PERSON_AND_ORGANIZATION ( #15518, #2538 ) ;
#9437 = CARTESIAN_POINT ( 'NONE',  ( -0.2144047338280713200, -0.2134821532158913959, 0.4137619532499328678 ) ) ;
#9438 =( BOUNDED_SURFACE ( )  B_SPLINE_SURFACE ( 3, 2, ( 
 ( #20896, #19184, #7964 ),
 ( #20776, #8203, #11397 ),
 ( #653, #290, #15416 ),
 ( #10055, #19308, #6380 ),
 ( #5897, #6013, #23071 ),
 ( #15176, #6133, #2493 ),
 ( #2376, #22844, #8081 ),
 ( #15532, #13600, #22955 ),
 ( #9564, #4191, #18829 ),
 ( #6257, #21013, #2611 ),
 ( #9686, #13481, #2252 ),
 ( #17479, #13717, #7730 ) ),
 .UNSPECIFIED., .F., .F., .T. ) 
 B_SPLINE_SURFACE_WITH_KNOTS ( ( 4, 2, 2, 2, 2, 4 ),
 ( 3, 3 ),
 ( 0.03744456216066675835, 0.04077857935059428507, 0.04244558794555804149, 0.04411259654052180484, 0.04744661373044932462, 0.05078063092037685133 ),
 ( 0.000000000000000000, 1.000000000000000000 ),
 .UNSPECIFIED. ) 
 GEOMETRIC_REPRESENTATION_ITEM ( )  RATIONAL_B_SPLINE_SURFACE ( (
 ( 1.000000000000000000, 0.8464669816041904271, 1.000000000000000000),
 ( 1.000000000000000000, 0.8515868425024901711, 1.000000000000000000),
 ( 1.000000000000000000, 0.8564835659287574066, 1.000000000000000000),
 ( 1.000000000000000000, 0.8619139284920220856, 1.000000000000000000),
 ( 1.000000000000000000, 0.8633991495534084626, 1.000000000000000000),
 ( 1.000000000000000000, 0.8654490525001213852, 1.000000000000000000),
 ( 1.000000000000000000, 0.8660089163969105774, 1.000000000000000000),
 ( 1.000000000000000000, 0.8660572738274425753, 1.000000000000000000),
 ( 1.000000000000000000, 0.8638780250325636123, 1.000000000000000000),
 ( 1.000000000000000000, 0.8566598902920686820, 1.000000000000000000),
 ( 1.000000000000000000, 0.8517009389554212051, 1.000000000000000000),
 ( 1.000000000000000000, 0.8464669816041904271, 1.000000000000000000) ) ) 
 REPRESENTATION_ITEM ( '' )  SURFACE ( )  );
#9439 = CARTESIAN_POINT ( 'NONE',  ( -0.1666460382175411203, 4.844395531962456758, 0.2656379378495577481 ) ) ;
#9440 = DIRECTION ( 'NONE',  ( -1.177540334020096140E-17, 0.2588190451025212946, -0.9659258262890679791 ) ) ;
#9441 = VERTEX_POINT ( 'NONE', #2653 ) ;
#9442 = CARTESIAN_POINT ( 'NONE',  ( -0.3119999999999999996, 0.4868055554038225874, 0.1292346314604056190 ) ) ;
#9443 = ORIENTED_EDGE ( 'NONE', *, *, #18738, .T. ) ;
#9444 = DIRECTION ( 'NONE',  ( 0.000000000000000000, 0.000000000000000000, -1.000000000000000000 ) ) ;
#9445 = CARTESIAN_POINT ( 'NONE',  ( 0.09335422435517687356, 4.763370768640803554, -0.2986308128854576194 ) ) ;
#9446 = CARTESIAN_POINT ( 'NONE',  ( 0.3613381517857143232, -0.009821428668970965531, 0.1174058825155742114 ) ) ;
#9447 = CARTESIAN_POINT ( 'NONE',  ( 3.857637417314162073E-17, 0.1199999999999999956, 0.3150000000000000022 ) ) ;
#9448 = ORIENTED_EDGE ( 'NONE', *, *, #16907, .F. ) ;
#9449 = CARTESIAN_POINT ( 'NONE',  ( -0.1116596296178199582, 0.03303571418817188854, -0.3436530038418508792 ) ) ;
#9450 = EDGE_LOOP ( 'NONE', ( #2998, #13811, #6724, #7399, #14255 ) ) ;
#9451 = LINE ( 'NONE', #22619, #11150 ) ;
#9452 = CARTESIAN_POINT ( 'NONE',  ( -0.2740703737067639589, 4.673339054025664296, 0.1502709304893539988 ) ) ;
#9453 = CARTESIAN_POINT ( 'NONE',  ( 0.1993543840281266633, 4.220916666742532186, -0.1993543840281266910 ) ) ;
#9454 = DIRECTION ( 'NONE',  ( -0.000000000000000000, -1.000000000000000000, -0.000000000000000000 ) ) ;
#9455 = CARTESIAN_POINT ( 'NONE',  ( -0.4687500000000004441, -0.2922835737772483400, 0.06112444011295366242 ) ) ;
#9456 = EDGE_CURVE ( 'NONE', #428, #795, #14417, .T. ) ;
#9457 = CARTESIAN_POINT ( 'NONE',  ( 0.3119999999999999996, 3.800777777777776478, -3.820898013339742174E-17 ) ) ;
#9458 = EDGE_CURVE ( 'NONE', #363, #23278, #4826, .T. ) ;
#9459 = CARTESIAN_POINT ( 'NONE',  ( 0.3119999999999999996, 4.693138889040620931, 0.1292346314604056190 ) ) ;
#9460 = AXIS2_PLACEMENT_3D ( 'NONE', #6656, #16294, #4591 ) ;
#9461 = CARTESIAN_POINT ( 'NONE',  ( 0.1167790944451424506, 5.106333333409199149, 0.2819296736111110424 ) ) ;
#9462 = CARTESIAN_POINT ( 'NONE',  ( -5.731347020009612645E-17, 0.3930555555555551583, 0.3119999999999999996 ) ) ;
#9463 = ORIENTED_EDGE ( 'NONE', *, *, #4838, .T. ) ;
#9464 = EDGE_CURVE ( 'NONE', #11636, #5331, #21588, .T. ) ;
#9465 = CARTESIAN_POINT ( 'NONE',  ( 1.791833110003796271E-17, 0.04312855400452411669, -0.2926285540045244216 ) ) ;
#9466 = VERTEX_POINT ( 'NONE', #14725 ) ;
#9467 = COORDINATED_UNIVERSAL_TIME_OFFSET ( 0, 0, .AHEAD. ) ;
#9468 = CARTESIAN_POINT ( 'NONE',  ( -0.3155070326520293400, 0.1306872919485614903, 0.3956250000000045564 ) ) ;
#9469 = CARTESIAN_POINT ( 'NONE',  ( 0.2819296736111110979, 5.154944444520308977, 0.1167790944451422425 ) ) ;
#9470 = CARTESIAN_POINT ( 'NONE',  ( -0.2819296736111110424, 3.759111111186976828, 0.1167790944451424923 ) ) ;
#9471 = CARTESIAN_POINT ( 'NONE',  ( 0.000000000000000000, 5.384999999999999787, -0.3119999999999999996 ) ) ;
#9472 = ADVANCED_FACE ( 'NONE', ( #20200 ), #22019, .T. ) ;
#9473 = B_SPLINE_CURVE_WITH_KNOTS ( 'NONE', 3,
 ( #719, #15360, #7471, #4257, #6082, #9877, #11708, #17306, #9753, #19489, #17190, #19374, #19131, #2435, #2671, #16742, #4372, #24, #8147, #6202, #839, #13668, #14920, #599, #8030, #21082 ),
 .UNSPECIFIED., .F., .F.,
 ( 4, 2, 2, 2, 2, 2, 2, 2, 2, 2, 2, 2, 4 ),
 ( 0.000000000000000000, 0.002383362014287317403, 0.004766724028574634807, 0.005958405035718294593, 0.007150086042861953511, 0.008341767050005612430, 0.009533448057149271349, 0.01191681007143659092, 0.01310849107858024984, 0.01430017208572390702, 0.01549185309286757115, 0.01668353410001123527, 0.01906689611429856004 ),
 .UNSPECIFIED. ) ;
#9474 = CARTESIAN_POINT ( 'NONE',  ( -6.979263641208234666E-17, 0.4044642856167431355, 0.3799334167787516425 ) ) ;
#9475 = CARTESIAN_POINT ( 'NONE',  ( -0.2764156081756484196, -0.1144950937579609362, -0.01930555555555453148 ) ) ;
#9476 = CARTESIAN_POINT ( 'NONE',  ( -0.1993543840281266633, 0.4034722221463555858, -0.1993543840281266910 ) ) ;
#9477 = CARTESIAN_POINT ( 'NONE',  ( -0.2764156081756484196, 0.1144950937579609918, 0.4251388888888933959 ) ) ;
#9478 = CARTESIAN_POINT ( 'NONE',  ( -0.1993543840281266355, 4.984805555631421470, 0.1993543840281267465 ) ) ;
#9479 = CARTESIAN_POINT ( 'NONE',  ( -0.009375000000009145115, -0.5358532185916164980, 0.06112444011295854046 ) ) ;
#9480 = CARTESIAN_POINT ( 'NONE',  ( 0.2819296736111110979, 4.880638888964754507, -3.452642723725051716E-17 ) ) ;
#9481 = CARTESIAN_POINT ( 'NONE',  ( 1.750236327630675475E-17, 0.05178571409062948661, -0.3999999999999999667 ) ) ;
#9482 = EDGE_CURVE ( 'NONE', #21880, #5470, #5318, .T. ) ;
#9483 = CARTESIAN_POINT ( 'NONE',  ( 0.8977114317029943891, 0.000000000000000000, -0.4292782587447178111 ) ) ;
#9484 = CARTESIAN_POINT ( 'NONE',  ( -1.399103805173478513E-17, 0.4635611116728546865, -1.084197934689580034 ) ) ;
#9485 = CARTESIAN_POINT ( 'NONE',  ( -0.1060554323913378977, 4.111524471938507119, -2.874935959385435336 ) ) ;
#9486 = CARTESIAN_POINT ( 'NONE',  ( -0.3119999999999999996, 4.495222222222221120, 0.000000000000000000 ) ) ;
#9487 = CARTESIAN_POINT ( 'NONE',  ( 0.1993543840281266633, 3.832027777853643791, -0.1993543840281266910 ) ) ;
#9488 = CARTESIAN_POINT ( 'NONE',  ( 0.3125000000000000000, 3.738758431839877614E-19, 0.4241666666666665253 ) ) ;
#9489 = DIRECTION ( 'NONE',  ( 8.659560562354947649E-17, -0.7071067811865464625, 0.7071067811865486830 ) ) ;
#9490 = CARTESIAN_POINT ( 'NONE',  ( -0.07694078045636083829, 3.736091107400131506, 0.3024941216908801911 ) ) ;
#9491 = CARTESIAN_POINT ( 'NONE',  ( 0.3039870060688493192, 4.583505726166830385, 0.07103347446430215151 ) ) ;
#9492 = VERTEX_POINT ( 'NONE', #11055 ) ;
#9493 = AXIS2_PLACEMENT_3D ( 'NONE', #16359, #18540, #18422 ) ;
#9494 = EDGE_CURVE ( 'NONE', #17972, #8797, #16365, .T. ) ;
#9495 = CYLINDRICAL_SURFACE ( 'NONE', #3693, 0.3150000000000000022 ) ;
#9496 = CARTESIAN_POINT ( 'NONE',  ( 0.04861964814276396873, 4.653546418008869701, -0.3084262645696678740 ) ) ;
#9497 = CARTESIAN_POINT ( 'NONE',  ( -0.2764156081756484196, 0.1144950937579609918, 0.3626388888888929518 ) ) ;
#9498 = CARTESIAN_POINT ( 'NONE',  ( -0.001116513862715997783, 3.932753884148758594, -0.3119982877432843082 ) ) ;
#9499 = CARTESIAN_POINT ( 'NONE',  ( 0.1797084794423411680, 3.735609856212664948, -0.2172307604343298448 ) ) ;
#9500 = VERTEX_POINT ( 'NONE', #21899 ) ;
#9501 = CARTESIAN_POINT ( 'NONE',  ( 0.3613381517857143232, 0.2937499999024575370, 0.1174058825155742114 ) ) ;
#9502 = CARTESIAN_POINT ( 'NONE',  ( 0.2819296736111110424, 0.4833333332574667462, -0.1167790944451423119 ) ) ;
#9503 = CARTESIAN_POINT ( 'NONE',  ( 0.1917372575570133186, 3.855115785418520513, 0.2494970157359910623 ) ) ;
#9504 = CARTESIAN_POINT ( 'NONE',  ( 0.4675994362856802367, -0.2849176297964606253, 0.04270874187135767497 ) ) ;
#9505 = CARTESIAN_POINT ( 'NONE',  ( 0.4593750000000003664, 0.2760455974562901482, 0.3779506566538943235 ) ) ;
#9506 = CARTESIAN_POINT ( 'NONE',  ( -0.1144950937579609918, -0.2764156081756484196, 0.1056944444444464504 ) ) ;
#9507 = AXIS2_PLACEMENT_3D ( 'NONE', #4370, #717, #15597 ) ;
#9508 = CARTESIAN_POINT ( 'NONE',  ( 0.3950000000000000178, 0.000000000000000000, -0.04999999999999918399 ) ) ;
#9509 = CARTESIAN_POINT ( 'NONE',  ( 0.3120000000000000551, 4.352861111111110404, 0.1292346314604056190 ) ) ;
#9510 = CARTESIAN_POINT ( 'NONE',  ( -0.3119999999999999996, 0.1604166666666663188, 0.1292346314604056190 ) ) ;
#9511 = CARTESIAN_POINT ( 'NONE',  ( 0.3119999999999999996, 5.193138888888888083, -0.1292346314604056745 ) ) ;
#9512 = B_SPLINE_CURVE_WITH_KNOTS ( 'NONE', 3,
 ( #9003, #92, #10964, #1802, #14498, #7179, #22287, #7420, #7059, #3391, #18389, #1684, #22045, #14621, #23858, #12684, #20102, #24109, #10843, #12805, #9247, #9119, #22165, #12932, #16447, #14750, #16688, #5341, #11081, #14871, #5581, #13047, #18272, #20224, #3514, #1924, #20463, #5466, #22406, #1568, #5707, #9370, #16811, #13170, #16567, #20342, #23989, #1447, #7301, #3630, #18510, #3760, #7536 ),
 .UNSPECIFIED., .F., .F.,
 ( 4, 2, 2, 2, 2, 2, 2, 2, 1, 1, 1, 2, 2, 2, 2, 2, 2, 2, 2, 2, 2, 2, 1, 1, 2, 2, 2, 2, 4 ),
 ( 0.7766889378257704202, 0.7778316968405288856, 0.7789744558552873510, 0.7801172148700458164, 0.7812599738848041708, 0.7824027328995626362, 0.7835454919143211017, 0.7838311816680106903, 0.7839026041064330874, 0.7839383153256442860, 0.7839561709352499408, 0.7839650987400527127, 0.7839740265448555956, 0.7841168714217005009, 0.7846882509290801222, 0.7858310099438394758, 0.7869737689585987184, 0.7881165279733580720, 0.7892592869881173145, 0.7904020460028766681, 0.7909734255102562894, 0.7911162703871011947, 0.7911876928255237029, 0.7912234040447349015, 0.7912412596543405563, 0.7912591152639461001, 0.7915448050176359107, 0.7926875640323953753, 0.7949730820619140825 ),
 .UNSPECIFIED. ) ;
#9513 = CARTESIAN_POINT ( 'NONE',  ( 0.1993543840281267465, 4.109805555631421470, 0.1993543840281266633 ) ) ;
#9514 = CARTESIAN_POINT ( 'NONE',  ( 0.3236067977499789694, 0.3839285712334865597, 0.2351141009169893659 ) ) ;
#9515 = EDGE_LOOP ( 'NONE', ( #15312, #9709, #16398, #17376, #21886 ) ) ;
#9516 = ORIENTED_EDGE ( 'NONE', *, *, #2272, .T. ) ;
#9517 = EDGE_CURVE ( 'NONE', #3616, #16166, #2301, .T. ) ;
#9518 = CARTESIAN_POINT ( 'NONE',  ( -0.2819296736111110424, 4.904944444520310753, -0.1167790944451423119 ) ) ;
#9519 = EDGE_CURVE ( 'NONE', #16287, #23361, #7424, .T. ) ;
#9520 = DIRECTION ( 'NONE',  ( 8.659560562354904508E-17, 0.7071067811865497932, -0.7071067811865452413 ) ) ;
#9521 = AXIS2_PLACEMENT_3D ( 'NONE', #8873, #4964, #6557 ) ;
#9522 = CARTESIAN_POINT ( 'NONE',  ( 0.000000000000000000, 0.000000000000000000, 0.000000000000000000 ) ) ;
#9523 = DIRECTION ( 'NONE',  ( -0.4999999999999978906, -0.8660254037844398178, 0.000000000000000000 ) ) ;
#9524 = DIRECTION ( 'NONE',  ( -0.000000000000000000, -1.000000000000000000, -0.000000000000000000 ) ) ;
#9525 = ADVANCED_FACE ( 'NONE', ( #20077 ), #19958, .F. ) ;
#9526 = CARTESIAN_POINT ( 'NONE',  ( -0.1993543840281266910, 4.623694444520309865, -0.1993543840281266910 ) ) ;
#9527 = CONTEXT_DEPENDENT_SHAPE_REPRESENTATION ( #8091, #16551 ) ;
#9528 = CARTESIAN_POINT ( 'NONE',  ( 0.2206173157302027954, 4.307722222222221120, -0.2206173157302028232 ) ) ;
#9529 = DIRECTION ( 'NONE',  ( 0.8660254037844443697, 0.000000000000000000, -0.4999999999999901745 ) ) ;
#9530 = CARTESIAN_POINT ( 'NONE',  ( 0.1167790944451423257, 0.4486111110352445364, -0.2819296736111110424 ) ) ;
#9531 = ORIENTED_EDGE ( 'NONE', *, *, #14815, .T. ) ;
#9532 = CARTESIAN_POINT ( 'NONE',  ( 0.1993543840281266910, 0.3340277777019111660, -0.1993543840281266910 ) ) ;
#9533 = CARTESIAN_POINT ( 'NONE',  ( 0.4200000000000000400, 2.689999999999999947, -2.566000000000000281 ) ) ;
#9534 = CARTESIAN_POINT ( 'NONE',  ( -3.827021247335479543E-17, -0.3125000000000000000, 0.1855555555555580272 ) ) ;
#9535 = CARTESIAN_POINT ( 'NONE',  ( 2.575339694675500462E-17, 0.2035714285714285143, -0.4205848896953069405 ) ) ;
#9536 = CARTESIAN_POINT ( 'NONE',  ( 0.1306872919485614071, -0.3155070326520293955, 0.02409722222222336965 ) ) ;
#9537 = CARTESIAN_POINT ( 'NONE',  ( -0.1591012008044459802, -0.4494087562524027857, 0.07655254331177707705 ) ) ;
#9538 = CYLINDRICAL_SURFACE ( 'NONE', #21801, 0.01874999999999999931 ) ;
#9539 = CARTESIAN_POINT ( 'NONE',  ( -0.1993543840281266633, 0.1673611110352444808, -0.1993543840281266910 ) ) ;
#9540 = CARTESIAN_POINT ( 'NONE',  ( 0.2819296736111110979, 0.2020833332574666907, 0.000000000000000000 ) ) ;
#9541 = CARTESIAN_POINT ( 'NONE',  ( 5.178964085587577574E-17, 4.269527777853643791, 0.2819296736111110979 ) ) ;
#9542 = CARTESIAN_POINT ( 'NONE',  ( 0.1236067977499789028, 0.1624999998049152239, 0.3804226065180614791 ) ) ;
#9543 = CONICAL_SURFACE ( 'NONE', #23146, 1.243000000000000105, 0.7853981633974551624 ) ;
#9544 = CARTESIAN_POINT ( 'NONE',  ( 5.178964085587577574E-17, 4.936194444520309865, 0.2819296736111110979 ) ) ;
#9545 = CC_DESIGN_PERSON_AND_ORGANIZATION_ASSIGNMENT ( #7636, #9834, ( #7598 ) ) ;
#9546 = CARTESIAN_POINT ( 'NONE',  ( 0.1993543840281266633, 4.387583333409199149, -0.1993543840281266910 ) ) ;
#9547 = CARTESIAN_POINT ( 'NONE',  ( 0.1988756632394131918, 3.704359868413474199, -0.2404006459456452249 ) ) ;
#9548 = VERTEX_POINT ( 'NONE', #4950 ) ;
#9549 = CARTESIAN_POINT ( 'NONE',  ( 5.463034709641816805E-17, 5.167344860100310910, 0.2973937581265823082 ) ) ;
#9550 = CARTESIAN_POINT ( 'NONE',  ( 0.1292346314604058410, 4.186194444596176290, 0.3119999999999998885 ) ) ;
#9551 = AXIS2_PLACEMENT_3D ( 'NONE', #2333, #19503, #17439 ) ;
#9552 = CARTESIAN_POINT ( 'NONE',  ( -5.731347020009612645E-17, 0.1152777777777774515, 0.3119999999999999996 ) ) ;
#9553 = CARTESIAN_POINT ( 'NONE',  ( -0.1419551320363411084, -0.2751926619867112178, -0.09836143147318530955 ) ) ;
#9554 = ORIENTED_EDGE ( 'NONE', *, *, #21779, .T. ) ;
#9555 = CALENDAR_DATE ( 2026, 7, 10 ) ;
#9556 = VECTOR ( 'NONE', #11211, 39.37007874015748143 ) ;
#9557 = CARTESIAN_POINT ( 'NONE',  ( -0.08048290441869994372, 4.847107040683704682, 0.3016807249711052075 ) ) ;
#9558 = CARTESIAN_POINT ( 'NONE',  ( -0.4466234456863258928, 1.658283848634127366, -2.678308925232197879 ) ) ;
#9559 = EDGE_CURVE ( 'NONE', #3584, #5059, #8728, .T. ) ;
#9560 = ORIENTED_EDGE ( 'NONE', *, *, #22713, .T. ) ;
#9561 = CARTESIAN_POINT ( 'NONE',  ( -0.3119999999999999996, 0.5354166665149336923, -0.1292346314604056745 ) ) ;
#9562 = VERTEX_POINT ( 'NONE', #12537 ) ;
#9563 = LINE ( 'NONE', #13005, #20688 ) ;
#9564 = CARTESIAN_POINT ( 'NONE',  ( 0.3068695747082215153, 0.3531079105191415324, 0.4306248051561324952 ) ) ;
#9565 = SPHERICAL_SURFACE ( 'NONE', #13644, 0.01874999999999999931 ) ;
#9566 = CARTESIAN_POINT ( 'NONE',  ( -0.2233192592356399442, 0.09017857133102905043, -0.3073725909049500049 ) ) ;
#9567 = DIRECTION ( 'NONE',  ( -0.000000000000000000, -1.000000000000000000, -0.000000000000000000 ) ) ;
#9568 = ORIENTED_EDGE ( 'NONE', *, *, #14593, .T. ) ;
#9569 = CC_DESIGN_SECURITY_CLASSIFICATION ( #5667, ( #11526 ) ) ;
#9570 = CARTESIAN_POINT ( 'NONE',  ( -0.2233192592356400275, 0.2008928570453147322, 0.3073725909049499494 ) ) ;
#9571 = DIRECTION ( 'NONE',  ( 0.000000000000000000, 0.000000000000000000, 1.000000000000000000 ) ) ;
#9572 = CARTESIAN_POINT ( 'NONE',  ( 0.000000000000000000, 0.000000000000000000, -0.1199999999999999956 ) ) ;
#9573 = CC_DESIGN_DATE_AND_TIME_ASSIGNMENT ( #10523, #4775, ( #21185 ) ) ;
#9574 = CARTESIAN_POINT ( 'NONE',  ( 0.2819296736111110979, 4.043833333409200037, 0.1167790944451422425 ) ) ;
#9575 = DIRECTION ( 'NONE',  ( 0.000000000000000000, 1.000000000000000000, 0.000000000000000000 ) ) ;
#9576 = CARTESIAN_POINT ( 'NONE',  ( 2.948500000000000121, 0.01249999999999952538, -0.03749999999999966555 ) ) ;
#9577 = CARTESIAN_POINT ( 'NONE',  ( -0.1292346314604057023, 3.783416666666665762, 0.3119999999999998885 ) ) ;
#9578 = CARTESIAN_POINT ( 'NONE',  ( 0.3119999999999999996, 4.811194444596175401, -0.1292346314604056745 ) ) ;
#9579 = CONICAL_SURFACE ( 'NONE', #14233, 0.3125000000000000000, 0.7853981633974497223 ) ;
#9580 = CARTESIAN_POINT ( 'NONE',  ( -0.1993543840281266355, 4.984805555631421470, 0.1993543840281267465 ) ) ;
#9581 = VERTEX_POINT ( 'NONE', #22140 ) ;
#9582 = CARTESIAN_POINT ( 'NONE',  ( -0.1167790944451423257, 4.286888888964754507, -0.2819296736111110424 ) ) ;
#9583 = CARTESIAN_POINT ( 'NONE',  ( 1.910449006669871087E-17, 0.4208333333333330040, -0.3119999999999999996 ) ) ;
#9584 = CARTESIAN_POINT ( 'NONE',  ( 0.3613381517857143232, 0.06517857133102902822, 0.000000000000000000 ) ) ;
#9585 = VERTEX_POINT ( 'NONE', #5438 ) ;
#9586 = LOCAL_TIME ( 21, 9, 13.00000000000000000, #1128 ) ;
#9587 = ORIENTED_EDGE ( 'NONE', *, *, #14542, .T. ) ;
#9588 = SHAPE_DEFINITION_REPRESENTATION ( #15937, #7952 ) ;
#9589 = VERTEX_POINT ( 'NONE', #3129 ) ;
#9590 = CYLINDRICAL_SURFACE ( 'NONE', #23920, 0.3125000000000000000 ) ;
#9591 = CARTESIAN_POINT ( 'NONE',  ( 0.1993543840281266633, 5.220916666742532186, -0.1993543840281266910 ) ) ;
#9592 = CARTESIAN_POINT ( 'NONE',  ( -0.1993543840281266355, 3.873694444520310309, 0.1993543840281267465 ) ) ;
#9593 = VECTOR ( 'NONE', #10101, 39.37007874015748143 ) ;
#9594 = LINE ( 'NONE', #17872, #17354 ) ;
#9595 = CARTESIAN_POINT ( 'NONE',  ( 0.4254231800974607736, -0.3089306822179591072, 0.05347271648849192399 ) ) ;
#9596 = EDGE_LOOP ( 'NONE', ( #12659, #13850, #22248, #13532, #6169, #14546, #22327, #15904, #716, #14084, #9383, #9704, #16896, #23974, #7329, #2380, #11541, #3434, #15726, #5387, #702, #2299, #484, #5289, #23906, #4118, #5069, #5850, #1156, #7257, #1955, #12012, #259, #19843, #4546, #17453, #4189, #6247, #11044, #12581, #8337, #2911, #5684, #4124, #23299, #94, #1086, #21373, #18501, #14163, #19887, #22712, #3461, #1030, #20215, #3836, #10796, #17295, #7728 ) ) ;
#9597 = CARTESIAN_POINT ( 'NONE',  ( 0.2764156081756484196, -5.077672346800151106E-17, 0.3383333333333372051 ) ) ;
#9598 = CARTESIAN_POINT ( 'NONE',  ( 0.2819296736111110424, 0.6013888888130223265, 0.1167790944451424923 ) ) ;
#9599 = CARTESIAN_POINT ( 'NONE',  ( -0.2764156081756484196, 0.1144950937579609918, 0.3695833333333374271 ) ) ;
#9600 = CARTESIAN_POINT ( 'NONE',  ( 0.1993543840281266633, 4.845916666742532186, -0.1993543840281266910 ) ) ;
#9601 = CARTESIAN_POINT ( 'NONE',  ( 0.009375000000000032613, -0.5358532185916218271, 0.06112444011295373875 ) ) ;
#9602 = ADVANCED_FACE ( 'NONE', ( #12906 ), #20319, .T. ) ;
#9603 = CARTESIAN_POINT ( 'NONE',  ( -0.2819296736111110424, 4.571611111186975940, -0.1167790944451423119 ) ) ;
#9604 = CARTESIAN_POINT ( 'NONE',  ( -0.2716011131362577880, 0.07493431514972544172, -0.07075596294687129528 ) ) ;
#9605 = CARTESIAN_POINT ( 'NONE',  ( 0.3141651762424315653, 4.863855663901686555, -0.02248318143069297226 ) ) ;
#9606 = CC_DESIGN_APPROVAL ( #19998, ( #15437 ) ) ;
#9607 = DIRECTION ( 'NONE',  ( -0.000000000000000000, 1.000000000000000000, -0.000000000000000000 ) ) ;
#9608 = CARTESIAN_POINT ( 'NONE',  ( 1.652571746775178152, 2.291712385858714285, -2.061529041877830704 ) ) ;
#9609 = CARTESIAN_POINT ( 'NONE',  ( -0.3119999999999999996, 4.550777777777777366, 0.000000000000000000 ) ) ;
#9610 = CARTESIAN_POINT ( 'NONE',  ( -0.2819296736111110979, 3.849388888964754507, -0.1167790944451422980 ) ) ;
#9611 = DIRECTION ( 'NONE',  ( -0.000000000000000000, -1.000000000000000000, -0.000000000000000000 ) ) ;
#9612 = CARTESIAN_POINT ( 'NONE',  ( 0.05926878199548974574, 4.986570782386274381, -0.3065401363359365750 ) ) ;
#9613 = ORIENTED_EDGE ( 'NONE', *, *, #6441, .F. ) ;
#9614 = VECTOR ( 'NONE', #21311, 39.37007874015748143 ) ;
#9615 = FACE_OUTER_BOUND ( 'NONE', #24054, .T. ) ;
#9616 = ORIENTED_EDGE ( 'NONE', *, *, #620, .F. ) ;
#9617 = CARTESIAN_POINT ( 'NONE',  ( -0.1584465904743051490, -0.4497866957027560897, 0.4135550951626319471 ) ) ;
#9618 = CARTESIAN_POINT ( 'NONE',  ( -3.863846776457871776E-17, -0.3155070326520292845, -0.1425694444444441933 ) ) ;
#9619 = ADVANCED_FACE ( 'NONE', ( #9223 ), #16662, .F. ) ;
#9620 = CARTESIAN_POINT ( 'NONE',  ( -0.0001593111292714336792, 3.932726740070024540, -0.3119999695236226889 ) ) ;
#9621 = CARTESIAN_POINT ( 'NONE',  ( 0.2876526673451095251, 5.142634612739459321, 0.1007097082411073097 ) ) ;
#9622 = VERTEX_POINT ( 'NONE', #6910 ) ;
#9623 = CARTESIAN_POINT ( 'NONE',  ( 0.1116596296178199027, -0.02053571438325667992, 0.3436530038418508792 ) ) ;
#9624 = CARTESIAN_POINT ( 'NONE',  ( -0.1167790944451424368, 0.5180555554796888451, 0.2819296736111110424 ) ) ;
#9625 = CARTESIAN_POINT ( 'NONE',  ( -0.1954553509668046918, -0.1954553509668046640, -0.1199999999999998013 ) ) ;
#9626 = CARTESIAN_POINT ( 'NONE',  ( 0.3048633063337730653, 0.3951878887010597530, -1.145478839108450941 ) ) ;
#9627 = CARTESIAN_POINT ( 'NONE',  ( 2.262531734667336369, 2.800838881557672355, -2.455161118442326984 ) ) ;
#9628 = CARTESIAN_POINT ( 'NONE',  ( 0.1144950937579609085, -0.2764156081756484751, 0.2793055555555589153 ) ) ;
#9629 = ADVANCED_FACE ( 'NONE', ( #3245 ), #10693, .F. ) ;
#9630 =( BOUNDED_CURVE ( )  B_SPLINE_CURVE ( 2, ( #10145, #17569, #859, #15744, #4636, #12102, #6102, #19512, #2805, #10260, #7819, #15262, #5981 ),
 .UNSPECIFIED., .F., .T. ) 
 B_SPLINE_CURVE_WITH_KNOTS ( ( 3, 2, 2, 2, 2, 2, 3 ),
 ( 0.6785714285714286031, 0.6857142857142857206, 0.6999999999999999556, 0.7142857142857143016, 0.7285714285714285365, 0.7428571428571428825, 0.7500000000000000000 ),
 .UNSPECIFIED. ) 
 CURVE ( )  GEOMETRIC_REPRESENTATION_ITEM ( )  RATIONAL_B_SPLINE_CURVE ( ( 0.9755282581475768211, 0.9755282581475769321, 1.000000000000000000, 0.9510565162951535312, 1.000000000000000000, 0.9510565162951535312, 1.000000000000000000, 0.9510565162951535312, 1.000000000000000000, 0.9510565162951535312, 1.000000000000000000, 0.9755282581475768211, 0.9755282581475768211 ) ) 
 REPRESENTATION_ITEM ( '' )  );
#9631 = PLANE ( 'NONE',  #20784 ) ;
#9632 =( BOUNDED_CURVE ( )  B_SPLINE_CURVE ( 2, ( #9004, #9248, #6935, #24110, #5467, #7302, #5212, #4972, #11082 ),
 .UNSPECIFIED., .F., .T. ) 
 B_SPLINE_CURVE_WITH_KNOTS ( ( 3, 2, 2, 2, 3 ),
 ( 0.5446428571428569843, 0.5491071428571427937, 0.5535714285714284921, 0.5580357142857141906, 0.5624999999999998890 ),
 .UNSPECIFIED. ) 
 CURVE ( )  GEOMETRIC_REPRESENTATION_ITEM ( )  RATIONAL_B_SPLINE_CURVE ( ( 1.000000000000001998, 0.9238795325112848511, 1.000000000000000000, 0.9238795325112867385, 1.000000000000000000, 0.9238795325112867385, 1.000000000000000000, 0.9238795325112886259, 0.9999999999999981126 ) ) 
 REPRESENTATION_ITEM ( '' )  );
#9633 = DIRECTION ( 'NONE',  ( 0.000000000000000000, 0.000000000000000000, -1.000000000000000000 ) ) ;
#9634 = CARTESIAN_POINT ( 'NONE',  ( -0.2206173157302027954, 0.2055555555555551861, -0.2206173157302028232 ) ) ;
#9635 = CARTESIAN_POINT ( 'NONE',  ( 0.3119999999999999996, 5.134111111111110404, -3.820898013339742174E-17 ) ) ;
#9636 = CARTESIAN_POINT ( 'NONE',  ( 0.2819296736111110424, 4.175777777853643791, -0.1167790944451423396 ) ) ;
#9637 = FACE_OUTER_BOUND ( 'NONE', #11577, .T. ) ;
#9638 = CARTESIAN_POINT ( 'NONE',  ( 0.000000000000000000, 0.000000000000000000, 1.326383476483184332 ) ) ;
#9639 = ORIENTED_EDGE ( 'NONE', *, *, #17817, .F. ) ;
#9640 = CARTESIAN_POINT ( 'NONE',  ( 0.1292346314604057300, 0.3409722222222218435, 0.3119999999999998885 ) ) ;
#9641 = CARTESIAN_POINT ( 'NONE',  ( 0.2819296736111110979, 4.880638888964754507, -3.452642723725051716E-17 ) ) ;
#9642 = CARTESIAN_POINT ( 'NONE',  ( 0.2923287055106771337, 0.4151785713310289228, 0.2123892367102621359 ) ) ;
#9643 = CARTESIAN_POINT ( 'NONE',  ( -0.2984124910806962849, 5.154444156555171297, -0.04193874527002016545 ) ) ;
#9644 = AXIS2_PLACEMENT_3D ( 'NONE', #19223, #9854, #87 ) ;
#9645 = CARTESIAN_POINT ( 'NONE',  ( 0.000000000000000000, 0.000000000000000000, 0.000000000000000000 ) ) ;
#9646 = CARTESIAN_POINT ( 'NONE',  ( 0.000000000000000000, 0.06786299768266475241, 0.000000000000000000 ) ) ;
#9647 = CARTESIAN_POINT ( 'NONE',  ( -0.2764156081756484196, -0.1144950937579609362, -0.1304166666666665420 ) ) ;
#9648 = CARTESIAN_POINT ( 'NONE',  ( -0.2819296736111110979, 4.255638888964754507, 0.000000000000000000 ) ) ;
#9649 = CALENDAR_DATE ( 2026, 7, 10 ) ;
#9650 = CARTESIAN_POINT ( 'NONE',  ( 1.726321361862525858E-17, 0.6187499999241333759, -0.2819296736111110979 ) ) ;
#9651 = PLANE ( 'NONE',  #17471 ) ;
#9652 = CARTESIAN_POINT ( 'NONE',  ( -5.178964085587577574E-17, 0.4243055554796889006, 0.2819296736111110979 ) ) ;
#9653 = ORIENTED_EDGE ( 'NONE', *, *, #22778, .F. ) ;
#9654 = CARTESIAN_POINT ( 'NONE',  ( 0.2819296736111110979, 0.4381944443685778512, 0.000000000000000000 ) ) ;
#9655 = DIRECTION ( 'NONE',  ( 0.000000000000000000, 0.000000000000000000, -1.000000000000000000 ) ) ;
#9656 = DIRECTION ( 'NONE',  ( 0.000000000000000000, 0.000000000000000000, -1.000000000000000000 ) ) ;
#9657 = CARTESIAN_POINT ( 'NONE',  ( -0.1236067977499789583, 0.2785714285714285254, -0.3804226065180614791 ) ) ;
#9658 = CARTESIAN_POINT ( 'NONE',  ( 0.3155070326520292290, -0.1306872919485616569, 0.08659722222222389354 ) ) ;
#9659 = EDGE_CURVE ( 'NONE', #5448, #21184, #18848, .T. ) ;
#9660 = DIRECTION ( 'NONE',  ( -0.000000000000000000, -1.000000000000000000, -0.000000000000000000 ) ) ;
#9661 = DIRECTION ( 'NONE',  ( 1.000000000000000000, 0.000000000000000000, 0.000000000000000000 ) ) ;
#9662 = CARTESIAN_POINT ( 'NONE',  ( -5.178964085587577574E-17, 0.5770833332574667462, 0.2819296736111110979 ) ) ;
#9663 = CARTESIAN_POINT ( 'NONE',  ( 1.726321361862525858E-17, 0.3270833332574666907, -0.2819296736111110979 ) ) ;
#9664 = CARTESIAN_POINT ( 'NONE',  ( -0.2819296736111110424, 4.314666666742533074, 0.1167790944451424923 ) ) ;
#9665 = TOROIDAL_SURFACE ( 'NONE', #5763, 0.3425000000000000266, 0.02999999999999999889 ) ;
#9666 = CARTESIAN_POINT ( 'NONE',  ( 2.575339694675500462E-17, 0.4089285712334865264, -0.4205848896953069405 ) ) ;
#9667 = CARTESIAN_POINT ( 'NONE',  ( 0.2819296736111110979, 4.891055555631421470, 0.1167790944451422425 ) ) ;
#9668 = CARTESIAN_POINT ( 'NONE',  ( -0.2819296736111110424, 4.523000000075865223, 0.1167790944451424923 ) ) ;
#9669 = LINE ( 'NONE', #18689, #884 ) ;
#9670 = VERTEX_POINT ( 'NONE', #1900 ) ;
#9671 = CARTESIAN_POINT ( 'NONE',  ( 0.000000000000000000, 2.689999999999999947, 0.000000000000000000 ) ) ;
#9672 = CARTESIAN_POINT ( 'NONE',  ( 5.731347020009612645E-17, 4.016055555707287006, 0.3119999999999999996 ) ) ;
#9673 = CARTESIAN_POINT ( 'NONE',  ( 3.063257713472607067E-17, 0.4197679491924312112, 0.2501339745962155581 ) ) ;
#9674 = APPLICATION_CONTEXT ( 'configuration controlled 3d designs of mechanical parts and assemblies' ) ;
#9675 = CARTESIAN_POINT ( 'NONE',  ( 0.1764095973160011710, -0.2469329051807456488, -0.09217807008012661452 ) ) ;
#9676 = ORIENTED_EDGE ( 'NONE', *, *, #18875, .T. ) ;
#9677 = AXIS2_PLACEMENT_3D ( 'NONE', #13001, #18465, #42 ) ;
#9678 = APPLICATION_PROTOCOL_DEFINITION ( 'international standard', 'config_control_design', 1994, #8883 ) ;
#9679 = CARTESIAN_POINT ( 'NONE',  ( 0.1695524133009104484, 0.2302630372892223998, 0.3969863378735464798 ) ) ;
#9680 = LINE ( 'NONE', #17119, #968 ) ;
#9681 = CARTESIAN_POINT ( 'NONE',  ( -0.2969134259396885023, 5.005069796490948519, 0.09796392844229065422 ) ) ;
#9682 = VERTEX_POINT ( 'NONE', #310 ) ;
#9683 = CARTESIAN_POINT ( 'NONE',  ( 0.3119999999999998885, 0.3965277776260449083, 0.1292346314604058410 ) ) ;
#9684 = EDGE_LOOP ( 'NONE', ( #11767, #12487, #1603, #14793, #17991 ) ) ;
#9685 = CARTESIAN_POINT ( 'NONE',  ( 0.0002138672942954442330, 4.266049809204471188, -0.3119999314205446073 ) ) ;
#9686 = CARTESIAN_POINT ( 'NONE',  ( 0.4208772603875943763, 0.2863811090245901303, 0.4064915563616229299 ) ) ;
#9687 = PLANE ( 'NONE',  #10520 ) ;
#9688 = CARTESIAN_POINT ( 'NONE',  ( -0.1116596296178199582, -0.05625000009754239222, -0.3436530038418508792 ) ) ;
#9689 = CARTESIAN_POINT ( 'NONE',  ( 0.01934007716052928150, 5.189873518840629529, -0.2887964054786675283 ) ) ;
#9690 = EDGE_CURVE ( 'NONE', #19937, #644, #7394, .T. ) ;
#9691 = EDGE_LOOP ( 'NONE', ( #24010, #18835, #3633, #20663 ) ) ;
#9692 = CARTESIAN_POINT ( 'NONE',  ( -0.3613381517857143788, 0.2651785713310289561, 0.1174058825155740310 ) ) ;
#9693 = CARTESIAN_POINT ( 'NONE',  ( -0.4500000000000003997, 0.2598076211353315124, 0.4425000000000000044 ) ) ;
#9694 = CARTESIAN_POINT ( 'NONE',  ( -0.2368270405986217797, 4.675129404167337022, 0.2031599927639998471 ) ) ;
#9695 = CARTESIAN_POINT ( 'NONE',  ( -0.1993543840281266910, 3.901472222298087544, -0.1993543840281266910 ) ) ;
#9696 = CARTESIAN_POINT ( 'NONE',  ( -0.1893589898698174179, -0.4210708385985257873, 0.4333520680959401239 ) ) ;
#9697 = CARTESIAN_POINT ( 'NONE',  ( 0.1963547988595201466, -0.4279003813870558282, 0.09139143879391149750 ) ) ;
#9698 = CARTESIAN_POINT ( 'NONE',  ( -0.3119999999999998885, 3.887583333333333613, 0.1292346314604058410 ) ) ;
#9699 = AXIS2_PLACEMENT_3D ( 'NONE', #14791, #3800, #3553 ) ;
#9700 = CARTESIAN_POINT ( 'NONE',  ( -0.2206173157302028232, 4.828555555707287894, -0.2206173157302028232 ) ) ;
#9701 = CARTESIAN_POINT ( 'NONE',  ( -0.2819296736111110424, 5.036888888964754507, 0.1167790944451424923 ) ) ;
#9702 = VERTEX_POINT ( 'NONE', #20557 ) ;
#9703 = CARTESIAN_POINT ( 'NONE',  ( 0.2819296736111110979, 4.321611111186976828, 0.1167790944451422425 ) ) ;
#9704 = ORIENTED_EDGE ( 'NONE', *, *, #22341, .F. ) ;
#9705 = CARTESIAN_POINT ( 'NONE',  ( -0.2923287055106771337, 0.1080357141881718719, 0.2123892367102619971 ) ) ;
#9706 = ORIENTED_EDGE ( 'NONE', *, *, #1423, .T. ) ;
#9707 = ORIENTED_EDGE ( 'NONE', *, *, #11413, .F. ) ;
#9708 = CALENDAR_DATE ( 2026, 7, 10 ) ;
#9709 = ORIENTED_EDGE ( 'NONE', *, *, #15835, .T. ) ;
#9710 = PRODUCT_DEFINITION ( 'UNKNOWN', '', #7598, #4357 ) ;
#9711 = CARTESIAN_POINT ( 'NONE',  ( 0.2230971623002953874, -0.2230971623002954429, 0.4199305555555602476 ) ) ;
#9712 = CARTESIAN_POINT ( 'NONE',  ( 0.000000000000000000, 3.659999999999999698, 0.000000000000000000 ) ) ;
#9713 = CARTESIAN_POINT ( 'NONE',  ( 0.2819296736111110979, 3.894527777853643347, -3.452642723725051716E-17 ) ) ;
#9714 = AXIS2_PLACEMENT_3D ( 'NONE', #4970, #12437, #3150 ) ;
#9715 = CARTESIAN_POINT ( 'NONE',  ( 0.08062935572735190071, 4.430412084064282219, -0.3015737216022094658 ) ) ;
#9716 = CARTESIAN_POINT ( 'NONE',  ( 5.731347020009612645E-17, 4.953555555555554157, 0.3119999999999999996 ) ) ;
#9717 = EDGE_LOOP ( 'NONE', ( #16273, #1248, #17843, #23840 ) ) ;
#9718 = CARTESIAN_POINT ( 'NONE',  ( 0.1144950937579611444, 0.2764156081756483641, 0.1820833333333359838 ) ) ;
#9719 = CARTESIAN_POINT ( 'NONE',  ( 0.2819296736111110424, 0.5458333332574668573, 0.1167790944451424923 ) ) ;
#9720 = CARTESIAN_POINT ( 'NONE',  ( -0.2764156081756484196, 1.692557448933383907E-17, -0.07833333333333278303 ) ) ;
#9721 = ORIENTED_EDGE ( 'NONE', *, *, #2323, .T. ) ;
#9722 = CARTESIAN_POINT ( 'NONE',  ( 0.1167790944451422702, 4.682722222298088433, -0.2819296736111110424 ) ) ;
#9723 = CARTESIAN_POINT ( 'NONE',  ( -0.1236067977499790416, 0.4410714283763437216, 0.3804226065180614236 ) ) ;
#9724 = CARTESIAN_POINT ( 'NONE',  ( 0.2819296736111110979, 4.602861111186975940, -3.452642723725051716E-17 ) ) ;
#9725 = CARTESIAN_POINT ( 'NONE',  ( -0.1841151976024358594, 0.2183016720772819608, -0.07412050734230554716 ) ) ;
#9726 = CARTESIAN_POINT ( 'NONE',  ( 0.2113513854172701378, 4.855985392576767978, 0.2295112932090857261 ) ) ;
#9727 = CARTESIAN_POINT ( 'NONE',  ( -0.2232596883534626875, -3.892158461848153852E-18, 0.3143945333366566230 ) ) ;
#9728 = CARTESIAN_POINT ( 'NONE',  ( 1.670753895751090790, 2.384778440500605168, -2.046330657626557858 ) ) ;
#9729 = CARTESIAN_POINT ( 'NONE',  ( -1.910449006669871087E-17, 4.592444444444443441, -0.3119999999999999996 ) ) ;
#9730 = CARTESIAN_POINT ( 'NONE',  ( -0.1167790944451423119, 3.731333333409198705, -0.2819296736111110979 ) ) ;
#9731 = CARTESIAN_POINT ( 'NONE',  ( -0.1236067977499790416, 0.2357142857142856818, 0.3804226065180614236 ) ) ;
#9732 = PERSON ( 'NAUO-PER1', 'UNSPECIFIED', 'UNSPECIFIED', ('UNSPECIFIED'), ('UNSPECIFIED'), ('UNSPECIFIED') ) ;
#9733 = VECTOR ( 'NONE', #16087, 39.37007874015748854 ) ;
#9734 = ORIENTED_EDGE ( 'NONE', *, *, #3221, .F. ) ;
#9735 = CARTESIAN_POINT ( 'NONE',  ( -0.2206173157302028232, 4.543833333333332725, -0.2206173157302028232 ) ) ;
#9736 = EDGE_LOOP ( 'NONE', ( #14598, #673, #17527, #5139, #1729, #6649, #8377 ) ) ;
#9737 = ADVANCED_FACE ( 'NONE', ( #22261 ), #15079, .F. ) ;
#9738 = CARTESIAN_POINT ( 'NONE',  ( 0.3121158769751342099, 4.697706800928946436, -0.04006652453352290560 ) ) ;
#9739 = ORIENTED_EDGE ( 'NONE', *, *, #18604, .F. ) ;
#9740 = EDGE_CURVE ( 'NONE', #11982, #11875, #8052, .T. ) ;
#9741 = CARTESIAN_POINT ( 'NONE',  ( 0.3088258284620388205, 4.642689360785702490, -0.05851397011192863151 ) ) ;
#9742 = CARTESIAN_POINT ( 'NONE',  ( 0.2764156081756484196, -5.077672346800151106E-17, 0.3938888888888931739 ) ) ;
#9743 = CARTESIAN_POINT ( 'NONE',  ( -0.0001528158053696555070, 3.932726555878094388, -0.3120000002100443703 ) ) ;
#9744 = ORIENTED_EDGE ( 'NONE', *, *, #13372, .T. ) ;
#9745 = CARTESIAN_POINT ( 'NONE',  ( -0.3613381517857144343, 0.1044642856167432993, 0.1174058825155740171 ) ) ;
#9746 = CARTESIAN_POINT ( 'NONE',  ( -0.2819296736111110979, 0.5111111110352446474, 0.1167790944451422425 ) ) ;
#9747 = CARTESIAN_POINT ( 'NONE',  ( 3.827021247335478926E-17, 6.000000000000000888, 0.3125000000000000555 ) ) ;
#9748 = CARTESIAN_POINT ( 'NONE',  ( 0.1399608807533026522, 0.7553615324114533180, -1.079965574340326917 ) ) ;
#9749 = LINE ( 'NONE', #9627, #17537 ) ;
#9750 = CARTESIAN_POINT ( 'NONE',  ( 0.1144950937579611444, 0.2764156081756483641, 0.07791666666666842433 ) ) ;
#9751 = CARTESIAN_POINT ( 'NONE',  ( -0.01019282354824687341, 5.118057215992540598, 0.3087295155953159731 ) ) ;
#9752 = DIRECTION ( 'NONE',  ( -0.6546536707079757544, -0.6546536707079760875, -0.3779644730092315830 ) ) ;
#9753 = CARTESIAN_POINT ( 'NONE',  ( -0.1023465816611775492, 2.632010880910606029E-18, -0.3732753122504546273 ) ) ;
#9754 = CARTESIAN_POINT ( 'NONE',  ( -0.1292346314604058410, 0.2784722222222218990, 0.3119999999999998885 ) ) ;
#9755 = CARTESIAN_POINT ( 'NONE',  ( -0.3119999999999998885, 5.165361111111110404, 0.1292346314604058410 ) ) ;
#9756 = CARTESIAN_POINT ( 'NONE',  ( -1.726321361862525858E-17, 4.130638888964754507, -0.2819296736111110979 ) ) ;
#9757 = CARTESIAN_POINT ( 'NONE',  ( -0.3120221670779859680, 4.334383852034481954, -0.04068519730541640678 ) ) ;
#9758 = DIRECTION ( 'NONE',  ( 0.8660254037844397068, 0.000000000000000000, -0.4999999999999979461 ) ) ;
#9759 = LINE ( 'NONE', #17197, #8698 ) ;
#9760 = EDGE_CURVE ( 'NONE', #14906, #13117, #22377, .T. ) ;
#9761 = VERTEX_POINT ( 'NONE', #18727 ) ;
#9762 = EDGE_CURVE ( 'NONE', #2014, #2791, #12699, .T. ) ;
#9763 = CARTESIAN_POINT ( 'NONE',  ( 0.2206173157302028232, 0.3583333333333329485, -0.2206173157302028232 ) ) ;
#9764 = CARTESIAN_POINT ( 'NONE',  ( 0.1993543840281266633, 4.832027777853643791, -0.1993543840281266910 ) ) ;
#9765 = CARTESIAN_POINT ( 'NONE',  ( 0.2923287055106771337, 0.3437499999024575814, 0.2123892367102621359 ) ) ;
#9766 = AXIS2_PLACEMENT_3D ( 'NONE', #10588, #18015, #19839 ) ;
#9767 = CARTESIAN_POINT ( 'NONE',  ( -0.02743319922242961131, 4.515305058140716810, 0.3107919259431392578 ) ) ;
#9768 = AXIS2_PLACEMENT_3D ( 'NONE', #14910, #139, #7582 ) ;
#9769 = ADVANCED_FACE ( 'NONE', ( #12740 ), #11017, .T. ) ;
#9770 = CARTESIAN_POINT ( 'NONE',  ( 1.573499999999982579, -0.7696290922066150175, -1.412500000000022959 ) ) ;
#9771 = DIRECTION ( 'NONE',  ( 0.000000000000000000, 1.000000000000000000, 0.000000000000000000 ) ) ;
#9772 = CARTESIAN_POINT ( 'NONE',  ( -0.3062750282812776725, 0.05890668782146677579, -0.09963899732724015856 ) ) ;
#9773 = CARTESIAN_POINT ( 'NONE',  ( -0.1993543840281266355, 4.207027777853643791, 0.1993543840281267465 ) ) ;
#9774 = CALENDAR_DATE ( 2026, 7, 10 ) ;
#9775 = CARTESIAN_POINT ( 'NONE',  ( -0.001030184878490023525, 4.043861028467455654, -0.3119985433042023470 ) ) ;
#9776 =( BOUNDED_CURVE ( )  B_SPLINE_CURVE ( 2, ( #21415, #17638, #18004 ),
 .UNSPECIFIED., .F., .T. ) 
 B_SPLINE_CURVE_WITH_KNOTS ( ( 3, 3 ),
 ( 0.8229166666666667407, 0.8267181212766938625 ),
 .UNSPECIFIED. ) 
 CURVE ( )  GEOMETRIC_REPRESENTATION_ITEM ( )  RATIONAL_B_SPLINE_CURVE ( ( 1.000000000000000000, 0.9722206238029704739, 0.9647168388458531307 ) ) 
 REPRESENTATION_ITEM ( '' )  );
#9777 = CARTESIAN_POINT ( 'NONE',  ( 0.2764156081756483641, 0.1144950937579610195, 0.07097222222222394905 ) ) ;
#9778 =( BOUNDED_CURVE ( )  B_SPLINE_CURVE ( 1, ( #1382, #10895 ),
 .UNSPECIFIED., .F., .F. ) 
 B_SPLINE_CURVE_WITH_KNOTS ( ( 2, 2 ),
 ( 0.000000000000000000, 1.000000000000000000 ),
 .UNSPECIFIED. ) 
 CURVE ( )  GEOMETRIC_REPRESENTATION_ITEM ( )  RATIONAL_B_SPLINE_CURVE ( ( 0.9836822358325096882, 0.9836822358325096882 ) ) 
 REPRESENTATION_ITEM ( '' )  );
#9779 = CARTESIAN_POINT ( 'NONE',  ( 0.000000000000000000, 0.000000000000000000, 0.000000000000000000 ) ) ;
#9780 = ORIENTED_EDGE ( 'NONE', *, *, #7098, .F. ) ;
#9781 = CARTESIAN_POINT ( 'NONE',  ( 1.726321361862525858E-17, 0.3965277777019111105, -0.2819296736111110979 ) ) ;
#9782 = DIRECTION ( 'NONE',  ( 0.000000000000000000, 0.000000000000000000, -1.000000000000000000 ) ) ;
#9783 = FACE_OUTER_BOUND ( 'NONE', #8715, .T. ) ;
#9784 = CARTESIAN_POINT ( 'NONE',  ( 0.2472135954999579166, 0.2464285714285713302, 0.3402603233408160732 ) ) ;
#9785 = CARTESIAN_POINT ( 'NONE',  ( -0.3155070326520293400, -0.1306872919485614626, 0.1768750000000023637 ) ) ;
#9786 = CARTESIAN_POINT ( 'NONE',  ( 0.000000000000000000, 5.384999999999999787, -0.3119999999999999996 ) ) ;
#9787 = ADVANCED_FACE ( 'NONE', ( #18 ), #11700, .F. ) ;
#9788 = CARTESIAN_POINT ( 'NONE',  ( -0.3882564258214251662, 2.740000000000000213, -0.6724798558878207766 ) ) ;
#9789 = B_SPLINE_CURVE_WITH_KNOTS ( 'NONE', 3,
 ( #19130, #718, #2200, #21201, #6322, #20962, #10001, #2315 ),
 .UNSPECIFIED., .F., .F.,
 ( 4, 2, 2, 4 ),
 ( 0.000000000000000000, 0.0004997454757086382867, 0.0007496182135629574301, 0.0009994909514172765734 ),
 .UNSPECIFIED. ) ;
#9790 = CARTESIAN_POINT ( 'NONE',  ( -0.2819296736111111534, 0.5666666665908000056, 0.1167790944451422563 ) ) ;
#9791 = CARTESIAN_POINT ( 'NONE',  ( -0.2819296736111110424, 0.1708333332574666907, -0.1167790944451423396 ) ) ;
#9792 = VECTOR ( 'NONE', #20042, 39.37007874015748143 ) ;
#9793 = CARTESIAN_POINT ( 'NONE',  ( 0.2819296736111110424, 4.398000000075866112, -0.1167790944451423396 ) ) ;
#9794 = CARTESIAN_POINT ( 'NONE',  ( 0.4000000000000000222, 0.3196428569477723358, 0.000000000000000000 ) ) ;
#9795 = CARTESIAN_POINT ( 'NONE',  ( -0.1993543840281266910, 4.804250000075865223, -0.1993543840281266910 ) ) ;
#9796 = CARTESIAN_POINT ( 'NONE',  ( 0.1167790944451422702, 4.224388888964755395, -0.2819296736111110979 ) ) ;
#9797 = CARTESIAN_POINT ( 'NONE',  ( -0.2209708691207961373, -0.2209708691207961095, 0.2966666666666704089 ) ) ;
#9798 = ORIENTED_EDGE ( 'NONE', *, *, #19239, .F. ) ;
#9799 = CARTESIAN_POINT ( 'NONE',  ( -0.04625313968440265822, 0.5145616147176192978, 0.07046346805509136335 ) ) ;
#9800 = CARTESIAN_POINT ( 'NONE',  ( -0.3119999999999998885, 3.783416666818399499, 0.1292346314604058410 ) ) ;
#9801 = CARTESIAN_POINT ( 'NONE',  ( -0.4000000000000000222, 0.2839285712334865819, -4.898587196589413075E-17 ) ) ;
#9802 = CARTESIAN_POINT ( 'NONE',  ( 0.2709282478163133612, -0.1304588658952313962, -0.08939837573807506155 ) ) ;
#9803 = ORIENTED_EDGE ( 'NONE', *, *, #6661, .T. ) ;
#9804 = B_SPLINE_CURVE_WITH_KNOTS ( 'NONE', 3,
 ( #662, #5789, #15543, #22966, #4435, #20670, #18840, #2136, #17008, #13365, #13959, #21269, #17977, #23200, #12503, #17727, #16022, #2734, #15896, #21627, #10431, #23559, #5035, #10543, #10062, #17855, #6749, #10185, #19554, #23439, #4920, #2845, #23318, #14194, #21503, #8331, #1022, #1268, #12384, #8585, #1146, #17609, #6511 ),
 .UNSPECIFIED., .F., .F.,
 ( 4, 2, 2, 2, 2, 2, 2, 2, 2, 2, 1, 1, 1, 2, 2, 2, 2, 2, 2, 2, 2, 2, 4 ),
 ( 0.1187879011222644082, 0.1199322595034874733, 0.1210766178847105384, 0.1222209762659336035, 0.1233653346471566686, 0.1245096930283797476, 0.1250818722189912802, 0.1253679618142970464, 0.1253858424140036620, 0.1253947827138569560, 0.1254037230137102499, 0.1254394842131234811, 0.1255110066119499157, 0.1256540514096028127, 0.1279427681720490539, 0.1302314849344952952, 0.1325202016969415364, 0.1348089184593877776, 0.1359532768406108982, 0.1360963216382637953, 0.1362393664359166645, 0.1365254560312224585, 0.1370976352218340188 ),
 .UNSPECIFIED. ) ;
#9805 = SECURITY_CLASSIFICATION_LEVEL ( 'unclassified' ) ;
#9806 = CARTESIAN_POINT ( 'NONE',  ( 0.4000000000000000222, 0.4624999998049150740, 0.000000000000000000 ) ) ;
#9807 = CARTESIAN_POINT ( 'NONE',  ( -0.5116234456863258950, 1.999640111863030478, -2.640781157734872320 ) ) ;
#9808 = ORIENTED_EDGE ( 'NONE', *, *, #1859, .F. ) ;
#9809 = CARTESIAN_POINT ( 'NONE',  ( -0.1993543840281266633, 0.01458333325746670114, -0.1993543840281266910 ) ) ;
#9810 = ORIENTED_EDGE ( 'NONE', *, *, #828, .F. ) ;
#9811 = CARTESIAN_POINT ( 'NONE',  ( 0.02913558044229962174, 4.265265441289421311, -0.3107272591473340118 ) ) ;
#9812 = CARTESIAN_POINT ( 'NONE',  ( 1.522235971340160240E-16, 0.01999999999999951469, 1.243000000000000105 ) ) ;
#9813 = CARTESIAN_POINT ( 'NONE',  ( -0.1292346314604058410, 0.5562499999999995781, 0.3119999999999998885 ) ) ;
#9814 = CARTESIAN_POINT ( 'NONE',  ( 0.3613381517857143232, 0.1401785713310289838, -0.1174058825155740587 ) ) ;
#9815 = CARTESIAN_POINT ( 'NONE',  ( -4.638126268221291196E-16, 0.1321428571428571175, -0.4000000000000000222 ) ) ;
#9816 = EDGE_LOOP ( 'NONE', ( #4178, #4446 ) ) ;
#9817 = CARTESIAN_POINT ( 'NONE',  ( 2.936000000000000387, 0.000000000000000000, -0.07500000000000014988 ) ) ;
#9818 = CARTESIAN_POINT ( 'NONE',  ( 1.887609879709022165, 2.740000000000000213, -2.645066201718798471 ) ) ;
#9819 = CARTESIAN_POINT ( 'NONE',  ( -0.3119999999999999996, 4.050777777777777366, 0.000000000000000000 ) ) ;
#9820 = CARTESIAN_POINT ( 'NONE',  ( -0.2819296736111110979, 4.019527777853642903, 0.000000000000000000 ) ) ;
#9821 = CARTESIAN_POINT ( 'NONE',  ( -0.3852690508743131792, -0.3188306871325582437, 0.4003899297375634325 ) ) ;
#9822 = CARTESIAN_POINT ( 'NONE',  ( 0.000000000000000000, 0.000000000000000000, 0.4425000000000000044 ) ) ;
#9823 = APPLICATION_CONTEXT ( 'configuration controlled 3d designs of mechanical parts and assemblies' ) ;
#9824 = CARTESIAN_POINT ( 'NONE',  ( 5.731347020009612645E-17, 4.738277777929510215, 0.3119999999999999996 ) ) ;
#9825 = CARTESIAN_POINT ( 'NONE',  ( 0.1167790944451422702, 4.960500000075865223, -0.2819296736111110979 ) ) ;
#9826 = ORIENTED_EDGE ( 'NONE', *, *, #15304, .F. ) ;
#9827 = CARTESIAN_POINT ( 'NONE',  ( -0.2819296736111110424, 4.293833333409199149, -0.1167790944451423119 ) ) ;
#9828 = ORIENTED_EDGE ( 'NONE', *, *, #19552, .T. ) ;
#9829 = EDGE_CURVE ( 'NONE', #19258, #10504, #9778, .T. ) ;
#9830 = CARTESIAN_POINT ( 'NONE',  ( -0.2233192592356400275, 0.04017857133102901990, 0.3073725909049499494 ) ) ;
#9831 = EDGE_CURVE ( 'NONE', #21366, #11205, #10779, .T. ) ;
#9832 = VERTEX_POINT ( 'NONE', #6991 ) ;
#9833 = VERTEX_POINT ( 'NONE', #18205 ) ;
#9834 = PERSON_AND_ORGANIZATION_ROLE ( 'creator' ) ;
#9835 = CARTESIAN_POINT ( 'NONE',  ( 0.3950000000000000178, 2.740039370078740433, -2.540999999999999925 ) ) ;
#9836 = CARTESIAN_POINT ( 'NONE',  ( 0.3119999999999999996, 0.2958333333333329485, 0.000000000000000000 ) ) ;
#9837 = ADVANCED_FACE ( 'NONE', ( #1501 ), #8936, .T. ) ;
#9838 = CARTESIAN_POINT ( 'NONE',  ( -0.2819296736111110979, 3.863277777853644235, -0.1167790944451422980 ) ) ;
#9839 = CARTESIAN_POINT ( 'NONE',  ( 0.1134877939392910096, 4.429446129279178912, -0.2906335559990496642 ) ) ;
#9840 = CARTESIAN_POINT ( 'NONE',  ( 0.3125000000000004996, 0.1294417382415917750, 0.2654166666666701313 ) ) ;
#9841 = CARTESIAN_POINT ( 'NONE',  ( 0.3838096539023117537, -0.3196732703672033327, 0.06591861138176849377 ) ) ;
#9842 = VERTEX_POINT ( 'NONE', #21977 ) ;
#9843 = CARTESIAN_POINT ( 'NONE',  ( -0.1144950937579609779, 0.2764156081756484196, 0.1334722222222244348 ) ) ;
#9844 = CARTESIAN_POINT ( 'NONE',  ( 0.1993543840281266910, 0.5006944443685779067, -0.1993543840281266910 ) ) ;
#9845 = CARTESIAN_POINT ( 'NONE',  ( 0.1954553509668047195, 0.1954553509668046085, 0.4077777777777821799 ) ) ;
#9846 = ORIENTED_EDGE ( 'NONE', *, *, #10241, .T. ) ;
#9847 = CARTESIAN_POINT ( 'NONE',  ( -0.2819296736111110979, 4.700083333409199149, 0.000000000000000000 ) ) ;
#9848 = CARTESIAN_POINT ( 'NONE',  ( -0.3119999999999999996, 3.936194444444443885, -0.1292346314604056468 ) ) ;
#9849 = AXIS2_PLACEMENT_3D ( 'NONE', #9484, #22524, #2045 ) ;
#9850 = CARTESIAN_POINT ( 'NONE',  ( -1.726321361862525858E-17, 4.727861111186976828, -0.2819296736111110979 ) ) ;
#9851 = DIRECTION ( 'NONE',  ( -0.000000000000000000, -0.9961946980917454342, 0.08715574274765830465 ) ) ;
#9852 = DIRECTION ( 'NONE',  ( 8.659560562354992023E-17, 0.7071067811865426878, -0.7071067811865523467 ) ) ;
#9853 = CYLINDRICAL_SURFACE ( 'NONE', #5932, 0.3119999999999999996 ) ;
#9854 = DIRECTION ( 'NONE',  ( -0.000000000000000000, -1.000000000000000000, -0.000000000000000000 ) ) ;
#9855 = CARTESIAN_POINT ( 'NONE',  ( 0.1292346314604056190, 4.255638888888888083, -0.3119999999999999996 ) ) ;
#9856 = CARTESIAN_POINT ( 'NONE',  ( -0.3236067977499789694, 0.2857142857142855874, -0.2351141009169893104 ) ) ;
#9857 = CARTESIAN_POINT ( 'NONE',  ( -0.1292346314604056190, 0.5284722220704892726, -0.3119999999999999996 ) ) ;
#9858 = CC_DESIGN_DATE_AND_TIME_ASSIGNMENT ( #2114, #20888, ( #2989 ) ) ;
#9859 = VERTEX_POINT ( 'NONE', #22217 ) ;
#9860 = CARTESIAN_POINT ( 'NONE',  ( 0.3108174967125439392, 4.584757462357911706, 0.02714687810677645849 ) ) ;
#9861 = ORIENTED_EDGE ( 'NONE', *, *, #15927, .F. ) ;
#9862 = CARTESIAN_POINT ( 'NONE',  ( 0.07869576298431067707, 4.684959685628617976, 0.3026069602474616982 ) ) ;
#9863 = VECTOR ( 'NONE', #21025, 39.37007874015748143 ) ;
#9864 = CARTESIAN_POINT ( 'NONE',  ( 0.4678838860311516079, -0.2663291305467024861, 0.05893128447555356919 ) ) ;
#9865 = CARTESIAN_POINT ( 'NONE',  ( -0.1144950937579609918, -0.2764156081756484196, 0.3765277777777820134 ) ) ;
#9866 = DIRECTION ( 'NONE',  ( -1.493785812010397745E-17, 1.000000000000000000, 0.000000000000000000 ) ) ;
#9867 = ORIENTED_EDGE ( 'NONE', *, *, #21809, .T. ) ;
#9868 = ADVANCED_FACE ( 'NONE', ( #5516 ), #5271, .F. ) ;
#9869 = CARTESIAN_POINT ( 'NONE',  ( -0.1116596296178200276, 0.4187499999024575370, 0.3436530038418508792 ) ) ;
#9870 = CARTESIAN_POINT ( 'NONE',  ( -0.1993543840281267465, 0.4590277777019111105, 0.1993543840281266633 ) ) ;
#9871 = FACE_OUTER_BOUND ( 'NONE', #9736, .T. ) ;
#9872 = CARTESIAN_POINT ( 'NONE',  ( 0.2082367465038017507, 0.2506576595349946368, -1.206325088425369563 ) ) ;
#9873 = CARTESIAN_POINT ( 'NONE',  ( 1.910449006669871087E-17, 0.5319444444444439979, -0.3119999999999999996 ) ) ;
#9874 = CARTESIAN_POINT ( 'NONE',  ( 0.1144950937579611444, 0.2764156081756483641, 0.2445833333333364279 ) ) ;
#9875 = FACE_OUTER_BOUND ( 'NONE', #14544, .T. ) ;
#9876 = CARTESIAN_POINT ( 'NONE',  ( 0.000000000000000000, 5.384999999999999787, -0.3119999999999999996 ) ) ;
#9877 = CARTESIAN_POINT ( 'NONE',  ( -0.1622275593423418982, 1.937136306180702348E-16, -0.3548286843789034140 ) ) ;
#9878 = CARTESIAN_POINT ( 'NONE',  ( -0.3119999999999999996, 0.2715277777777774793, 0.1292346314604056190 ) ) ;
#9879 = CARTESIAN_POINT ( 'NONE',  ( 0.1292346314604056190, 4.866749999999999687, -0.3119999999999999996 ) ) ;
#9880 = AXIS2_PLACEMENT_3D ( 'NONE', #9779, #622, #10025 ) ;
#9881 = EDGE_CURVE ( 'NONE', #14569, #11335, #2349, .T. ) ;
#9882 = CARTESIAN_POINT ( 'NONE',  ( -0.1167790944451423257, 4.189666666742533074, -0.2819296736111110424 ) ) ;
#9883 = CARTESIAN_POINT ( 'NONE',  ( 0.4449999999999992295, 0.000000000000000000, -0.04999999999999918399 ) ) ;
#9884 = CARTESIAN_POINT ( 'NONE',  ( -0.4208308994021711102, 0.2864083541825031554, 0.4065068718547070747 ) ) ;
#9885 = PLANE ( 'NONE',  #22323 ) ;
#9886 = ORIENTED_EDGE ( 'NONE', *, *, #3485, .T. ) ;
#9887 = FACE_OUTER_BOUND ( 'NONE', #17223, .T. ) ;
#9888 = CARTESIAN_POINT ( 'NONE',  ( 5.178964085587577574E-17, 4.755638888964754507, 0.2819296736111110979 ) ) ;
#9889 = CARTESIAN_POINT ( 'NONE',  ( -0.2233192592356399442, 0.3758928570453146656, -0.3073725909049499494 ) ) ;
#9890 = CARTESIAN_POINT ( 'NONE',  ( -0.05588801071484209709, 4.514508298373136164, 0.3071457712218207403 ) ) ;
#9891 = CALENDAR_DATE ( 2026, 7, 10 ) ;
#9892 = FACE_OUTER_BOUND ( 'NONE', #1758, .T. ) ;
#9893 = CARTESIAN_POINT ( 'NONE',  ( 0.1167790944451424506, 4.273000000075865223, 0.2819296736111110424 ) ) ;
#9894 = APPROVAL_ROLE ( '' ) ;
#9895 = AXIS2_PLACEMENT_3D ( 'NONE', #2586, #8175, #19159 ) ;
#9896 = CARTESIAN_POINT ( 'NONE',  ( -0.2983136309931767038, 4.055085950308684239, -0.09350340892401856618 ) ) ;
#9897 = DIRECTION ( 'NONE',  ( 0.4999999999999901745, -0.000000000000000000, 0.8660254037844443697 ) ) ;
#9898 = CARTESIAN_POINT ( 'NONE',  ( 0.3125000000000000000, -5.740531871003217465E-17, 0.3730555555555599145 ) ) ;
#9899 = CARTESIAN_POINT ( 'NONE',  ( -0.2819296736111110979, 0.3548611110352445364, -3.452642723725051716E-17 ) ) ;
#9900 = FACE_OUTER_BOUND ( 'NONE', #23941, .T. ) ;
#9901 = CARTESIAN_POINT ( 'NONE',  ( -0.4593750000000004219, 0.2760455974562897596, 0.06112444011295372487 ) ) ;
#9902 = DIRECTION ( 'NONE',  ( -0.000000000000000000, -1.000000000000000000, -0.000000000000000000 ) ) ;
#9903 = CARTESIAN_POINT ( 'NONE',  ( -0.3155070326520292845, 1.931923388228935888E-17, 0.1178472222222241295 ) ) ;
#9904 = CARTESIAN_POINT ( 'NONE',  ( 0.000000000000000000, 5.500232050807569273, 0.000000000000000000 ) ) ;
#9905 = CARTESIAN_POINT ( 'NONE',  ( 0.3119999999999999996, 5.022999999999999687, -3.820898013339742174E-17 ) ) ;
#9906 = CARTESIAN_POINT ( 'NONE',  ( 1.726321361862525858E-17, 0.5493055554796888451, -0.2819296736111110979 ) ) ;
#9907 = CARTESIAN_POINT ( 'NONE',  ( 0.1167790944451423535, 0.1916666665908000333, 0.2819296736111110424 ) ) ;
#9908 = CARTESIAN_POINT ( 'NONE',  ( 5.178964085587577574E-17, 4.213972222298087544, 0.2819296736111110979 ) ) ;
#9909 = CARTESIAN_POINT ( 'NONE',  ( 0.1236067977499789028, 0.2339285712334865930, 0.3804226065180614791 ) ) ;
#9910 = EDGE_CURVE ( 'NONE', #24096, #16027, #20752, .T. ) ;
#9911 = CARTESIAN_POINT ( 'NONE',  ( -0.2819296736111110424, 4.870222222298087544, 0.1167790944451424923 ) ) ;
#9912 = DIRECTION ( 'NONE',  ( -0.4999999999999916178, 0.000000000000000000, 0.8660254037844433705 ) ) ;
#9913 = ORIENTED_EDGE ( 'NONE', *, *, #10920, .F. ) ;
#9914 = CARTESIAN_POINT ( 'NONE',  ( 0.1292346314604095325, 4.512583333333333613, 0.3119999999999962248 ) ) ;
#9915 = CARTESIAN_POINT ( 'NONE',  ( 0.2206173157302027954, 3.759111111262843696, -0.2206173157302028232 ) ) ;
#9916 = CONICAL_SURFACE ( 'NONE', #7570, 0.2041999999999999926, 0.7853981633974621568 ) ;
#9917 = CARTESIAN_POINT ( 'NONE',  ( -1.910449006669871087E-17, 4.759111111111110404, -0.3119999999999999996 ) ) ;
#9918 = SHAPE_REPRESENTATION_RELATIONSHIP ( 'NONE' , 'NONE' ,  #1861, #19865 ) ;
#9919 = ORIENTED_EDGE ( 'NONE', *, *, #4050, .F. ) ;
#9920 =( BOUNDED_CURVE ( )  B_SPLINE_CURVE ( 2, ( #2097, #7825, #20988, #11739, #9905, #3810, #630, #13453, #4165 ),
 .UNSPECIFIED., .F., .T. ) 
 B_SPLINE_CURVE_WITH_KNOTS ( ( 3, 2, 2, 2, 3 ),
 ( 0.1517857142857139685, 0.1562499999999997780, 0.1607142857142855874, 0.1651785714285713969, 0.1696428571428572063 ),
 .UNSPECIFIED. ) 
 CURVE ( )  GEOMETRIC_REPRESENTATION_ITEM ( )  RATIONAL_B_SPLINE_CURVE ( ( 1.000000000000005107, 0.9238795325112815204, 1.000000000000000000, 0.9238795325112867385, 1.000000000000000000, 0.9238795325112867385, 1.000000000000000000, 0.9238795325112857393, 1.000000000000000888 ) ) 
 REPRESENTATION_ITEM ( '' )  );
#9921 = VECTOR ( 'NONE', #22083, 39.37007874015748854 ) ;
#9922 = APPLICATION_PROTOCOL_DEFINITION ( 'international standard', 'config_control_design', 1994, #1723 ) ;
#9923 = DIRECTION ( 'NONE',  ( -0.08715574274765833240, 0.9961946980917454342, 3.870492493070290181E-17 ) ) ;
#9924 = ADVANCED_FACE ( 'NONE', ( #18681 ), #23351, .T. ) ;
#9925 = CARTESIAN_POINT ( 'NONE',  ( -0.5116234456863258950, 5.071846480923145606, -2.640781157734872320 ) ) ;
#9926 = ORIENTED_EDGE ( 'NONE', *, *, #7985, .F. ) ;
#9927 = CARTESIAN_POINT ( 'NONE',  ( -0.2819296736111110424, 0.1847222221463555858, -0.1167790944451423396 ) ) ;
#9928 = EDGE_CURVE ( 'NONE', #19328, #19011, #5989, .T. ) ;
#9929 = EDGE_CURVE ( 'NONE', #13004, #8463, #17043, .T. ) ;
#9930 = VERTEX_POINT ( 'NONE', #5637 ) ;
#9931 = CARTESIAN_POINT ( 'NONE',  ( 0.0001053197333313014172, 4.266052725934510903, -0.3119999869445473362 ) ) ;
#9932 = CARTESIAN_POINT ( 'NONE',  ( -1.910449006669871087E-17, 4.647999999999998799, -0.3119999999999999996 ) ) ;
#9933 = VECTOR ( 'NONE', #2083, 39.37007874015748143 ) ;
#9934 = CARTESIAN_POINT ( 'NONE',  ( 0.3613381517857143232, 0.2758928570453146878, 0.1174058825155742114 ) ) ;
#9935 = CARTESIAN_POINT ( 'NONE',  ( 0.1304432934080578810, 5.186978988233328813, -0.2602171520964869922 ) ) ;
#9936 = ORIENTED_EDGE ( 'NONE', *, *, #2323, .F. ) ;
#9937 = CARTESIAN_POINT ( 'NONE',  ( 0.3950000000000000733, 0.04999999999999864969, -0.4043744331762961775 ) ) ;
#9938 = CARTESIAN_POINT ( 'NONE',  ( -0.1552113907098449930, 4.678091210889574469, 0.2737309952764502285 ) ) ;
#9939 = ADVANCED_FACE ( 'NONE', ( #4043 ), #13330, .F. ) ;
#9940 = CARTESIAN_POINT ( 'NONE',  ( -0.2819296736111110424, 4.016055555631421470, -0.1167790944451423119 ) ) ;
#9941 = CARTESIAN_POINT ( 'NONE',  ( -0.01607592287031538517, 0.03839369622198421372, 0.2878936962219845741 ) ) ;
#9942 = LOCAL_TIME ( 21, 9, 13.00000000000000000, #17919 ) ;
#9943 = DIRECTION ( 'NONE',  ( 0.5000000000000012212, -0.8660254037844380415, 0.000000000000000000 ) ) ;
#9944 = CARTESIAN_POINT ( 'NONE',  ( 0.3119999999999999996, 4.477861111262843252, -0.1292346314604056745 ) ) ;
#9945 = CARTESIAN_POINT ( 'NONE',  ( -0.2819296736111110979, 4.866750000075866112, 0.000000000000000000 ) ) ;
#9946 = ORIENTED_EDGE ( 'NONE', *, *, #19742, .F. ) ;
#9947 = CARTESIAN_POINT ( 'NONE',  ( -0.1993543840281266355, 4.026472222298087544, 0.1993543840281267465 ) ) ;
#9948 = ORIENTED_EDGE ( 'NONE', *, *, #22173, .T. ) ;
#9949 = CARTESIAN_POINT ( 'NONE',  ( -6.979263641208234666E-17, 0.2616071427596003973, 0.3799334167787516980 ) ) ;
#9950 = VECTOR ( 'NONE', #22176, 39.37007874015747433 ) ;
#9951 = ORIENTED_EDGE ( 'NONE', *, *, #4975, .T. ) ;
#9952 = ORIENTED_EDGE ( 'NONE', *, *, #11865, .F. ) ;
#9953 = CALENDAR_DATE ( 2026, 7, 10 ) ;
#9954 = ORIENTED_EDGE ( 'NONE', *, *, #6032, .T. ) ;
#9955 = CYLINDRICAL_SURFACE ( 'NONE', #19652, 0.3125000000000000000 ) ;
#9956 = CARTESIAN_POINT ( 'NONE',  ( 0.000000000000000000, 3.700000000000000622, 0.000000000000000000 ) ) ;
#9957 = CC_DESIGN_APPROVAL ( #14947, ( #2554 ) ) ;
#9958 = CARTESIAN_POINT ( 'NONE',  ( 0.2206173157302028232, 0.1291666665149337201, -0.2206173157302028232 ) ) ;
#9959 = PLANE ( 'NONE',  #6052 ) ;
#9960 = CARTESIAN_POINT ( 'NONE',  ( -0.3124999999999993894, 0.1294417382415927742, 0.2862500000000035572 ) ) ;
#9961 = CARTESIAN_POINT ( 'NONE',  ( -0.1292346314604112256, 4.929250000000000576, -0.3119999999999945040 ) ) ;
#9962 = CARTESIAN_POINT ( 'NONE',  ( -0.2764156081756484196, -0.1144950937579609362, 0.3140277777777815138 ) ) ;
#9963 = CARTESIAN_POINT ( 'NONE',  ( -0.2819296736111110979, 0.5770833332574666352, -3.452642723725051716E-17 ) ) ;
#9964 = CARTESIAN_POINT ( 'NONE',  ( 0.2764156081756484196, -5.077672346800151106E-17, 0.4008333333333376491 ) ) ;
#9965 = EDGE_CURVE ( 'NONE', #8097, #11233, #9920, .T. ) ;
#9966 = ORIENTED_EDGE ( 'NONE', *, *, #20471, .F. ) ;
#9967 = CARTESIAN_POINT ( 'NONE',  ( -0.2819296736111110424, 4.807722222298088433, -0.1167790944451423119 ) ) ;
#9968 = CARTESIAN_POINT ( 'NONE',  ( 0.6107956263425956545, 2.685901063997346405, -1.186814756611144883 ) ) ;
#9969 = VECTOR ( 'NONE', #21469, 39.37007874015748143 ) ;
#9970 = EDGE_CURVE ( 'NONE', #6278, #23184, #11496, .T. ) ;
#9971 = CARTESIAN_POINT ( 'NONE',  ( 0.2819296736111110979, 4.713972222298087544, -3.452642723725051716E-17 ) ) ;
#9972 = CARTESIAN_POINT ( 'NONE',  ( -0.004450248486120969398, 4.155072206286953396, -0.3119727959386125460 ) ) ;
#9973 = CARTESIAN_POINT ( 'NONE',  ( -3.827021247335479543E-17, -0.3125000000000000000, 0.3522222222222260446 ) ) ;
#9974 = DIRECTION ( 'NONE',  ( 8.659560562354915602E-17, -0.7071067811865489050, 0.7071067811865461294 ) ) ;
#9975 = CARTESIAN_POINT ( 'NONE',  ( -0.4687500000000003886, 0.2598076211353315124, 0.06112444011295379426 ) ) ;
#9976 = CARTESIAN_POINT ( 'NONE',  ( 0.2206173157302028787, 4.238277777777777366, 0.2206173157302027954 ) ) ;
#9977 = B_SPLINE_CURVE_WITH_KNOTS ( 'NONE', 3,
 ( #5131, #5252, #8921, #5375, #12723, #18426, #20262, #16244, #12596, #14536, #10759, #14291, #1244, #1363, #16121, #6728, #23655, #10635, #21841, #20016, #18189, #20138, #16364, #21728, #3303, #23895, #3428, #10879, #18308, #22079, #1606, #21602, #9040, #9158, #23774, #3547, #14171, #16485, #12841, #10999, #7213, #4896, #1719, #8669, #23417, #12358, #19777, #3073, #23535, #6851, #12475, #19896, #3186, #13315, #20614, #20734, #3912, #4028, #15019 ),
 .UNSPECIFIED., .F., .F.,
 ( 4, 2, 1, 1, 1, 1, 1, 2, 2, 2, 2, 2, 2, 2, 2, 1, 2, 2, 2, 2, 2, 2, 2, 2, 2, 1, 2, 2, 1, 1, 2, 2, 2, 4 ),
 ( 0.6670385189161691653, 0.6670429817324019517, 0.6670474445486348491, 0.6670563701811004220, 0.6670742214460316788, 0.6671099239758941923, 0.6671813290356192194, 0.6673241391550693846, 0.6676097593939694930, 0.6681809998717698207, 0.6693234808273704761, 0.6704659617829711316, 0.6716084427385717870, 0.6718940629774720064, 0.6719654680371970334, 0.6720368730969220605, 0.6721796832163722257, 0.6727509236941725534, 0.6738934046497732089, 0.6750358856053739753, 0.6761783665609747418, 0.6773208475165753972, 0.6784633284721761637, 0.6790345689499764914, 0.6793201891888767108, 0.6793915942486017379, 0.6794094455135329946, 0.6794183711459985675, 0.6794272967784642514, 0.6794629993083267649, 0.6796058094277768191, 0.6807482903833775856, 0.6830332522945791185, 0.6853182142057806514 ),
 .UNSPECIFIED. ) ;
#9978 = CARTESIAN_POINT ( 'NONE',  ( -0.3119999999999999996, 5.165361111262843252, -0.1292346314604056468 ) ) ;
#9979 = CARTESIAN_POINT ( 'NONE',  ( -1.910449006669871087E-17, 3.981333333333332725, -0.3119999999999999996 ) ) ;
#9980 = PRODUCT_DEFINITION_FORMATION_WITH_SPECIFIED_SOURCE ( 'ANY', '', #19837, .NOT_KNOWN. ) ;
#9981 = VERTEX_POINT ( 'NONE', #19047 ) ;
#9982 = CARTESIAN_POINT ( 'NONE',  ( 0.009374999999999774139, 0.5358532185916217161, 0.06112444011295372487 ) ) ;
#9983 = EDGE_LOOP ( 'NONE', ( #9123, #122, #10090, #17303 ) ) ;
#9984 = CARTESIAN_POINT ( 'NONE',  ( 0.2209708691207961095, -0.2209708691207961651, 0.08833333333333540094 ) ) ;
#9985 = AXIS2_PLACEMENT_3D ( 'NONE', #10046, #762, #10285 ) ;
#9986 = DESIGN_CONTEXT ( 'detailed design', #2977, 'design' ) ;
#9987 = AXIS2_PLACEMENT_3D ( 'NONE', #2015, #11650, #535 ) ;
#9988 = CARTESIAN_POINT ( 'NONE',  ( 0.1978063296366817103, 4.133267444897331444, 0.2413868729338500829 ) ) ;
#9989 = CARTESIAN_POINT ( 'NONE',  ( -0.1144950937579609779, 0.2764156081756484196, 0.4668055555555604141 ) ) ;
#9990 = CARTESIAN_POINT ( 'NONE',  ( -0.002233241627982304571, 3.932785552190646516, -0.3119931493891720531 ) ) ;
#9991 = ORGANIZATION ( 'NAUO-ORG5', 'UNSPECIFIED', 'UNSPECIFIED' ) ;
#9992 = CARTESIAN_POINT ( 'NONE',  ( -6.979263641208234666E-17, 0.04732142847388615819, 0.3799334167787516425 ) ) ;
#9993 = CARTESIAN_POINT ( 'NONE',  ( 0.1167790944451423257, 0.3791666665908000611, -0.2819296736111110424 ) ) ;
#9994 = DIRECTION ( 'NONE',  ( -0.000000000000000000, 1.000000000000000000, 0.000000000000000000 ) ) ;
#9995 = CARTESIAN_POINT ( 'NONE',  ( 2.108637995767629114, 2.978485840173427324, -1.763529041877836434 ) ) ;
#9996 = CARTESIAN_POINT ( 'NONE',  ( 0.006672437742759138729, 0.5374135436383427056, 0.05975564523638855763 ) ) ;
#9997 = CARTESIAN_POINT ( 'NONE',  ( -0.2764156081756484196, -0.1144950937579609362, 0.1543055555555579716 ) ) ;
#9998 = ORIENTED_EDGE ( 'NONE', *, *, #16381, .T. ) ;
#9999 = ADVANCED_FACE ( 'NONE', ( #267 ), #18931, .F. ) ;
#10000 = CARTESIAN_POINT ( 'NONE',  ( -0.1765272216824294027, 4.621815342127092663, 0.2574651026513284924 ) ) ;
#10001 = CARTESIAN_POINT ( 'NONE',  ( -0.01571427698143878018, 0.5457913482617613443, 0.04342012612512791830 ) ) ;
#10002 = CARTESIAN_POINT ( 'NONE',  ( 5.731347020009612645E-17, 4.731333333333332725, 0.3119999999999999996 ) ) ;
#10003 = CARTESIAN_POINT ( 'NONE',  ( 0.3119999999999999996, 0.1847222222222218990, 0.000000000000000000 ) ) ;
#10004 = CARTESIAN_POINT ( 'NONE',  ( -0.3119999999999999996, 4.991749999999999687, -0.1292346314604056468 ) ) ;
#10005 = VECTOR ( 'NONE', #23390, 39.37007874015748854 ) ;
#10006 = CARTESIAN_POINT ( 'NONE',  ( -0.2819296736111110979, 3.922305555631421914, 0.000000000000000000 ) ) ;
#10007 = CARTESIAN_POINT ( 'NONE',  ( -0.4687500000000003886, 0.2706329386826371031, 0.4425000000000000044 ) ) ;
#10008 = CARTESIAN_POINT ( 'NONE',  ( -0.1580560128843782330, 0.4500121957794397942, 0.4142946745564982658 ) ) ;
#10009 = CARTESIAN_POINT ( 'NONE',  ( 0.3117612485122355781, 4.807384657386537086, 0.01257049743255786618 ) ) ;
#10010 = ORIENTED_EDGE ( 'NONE', *, *, #34, .F. ) ;
#10011 = CYLINDRICAL_SURFACE ( 'NONE', #20239, 0.3119999999999999996 ) ;
#10012 = CARTESIAN_POINT ( 'NONE',  ( 0.2819296736111110979, 4.658416666742532186, -3.452642723725051716E-17 ) ) ;
#10013 = CARTESIAN_POINT ( 'NONE',  ( 0.09136153228682411531, 0.5015293579687603032, 0.06108838700204547584 ) ) ;
#10014 = ADVANCED_FACE ( 'NONE', ( #22819 ), #6109, .F. ) ;
#10015 = CARTESIAN_POINT ( 'NONE',  ( -0.1834827640909514057, 5.162357905306088846, 0.2362001855642932580 ) ) ;
#10016 = CARTESIAN_POINT ( 'NONE',  ( -0.4687500000000003886, 0.08695190463377312773, 0.07654938221781626417 ) ) ;
#10017 = LINE ( 'NONE', #8164, #9933 ) ;
#10018 = AXIS2_PLACEMENT_3D ( 'NONE', #12610, #1496, #8931 ) ;
#10019 = DIRECTION ( 'NONE',  ( -0.08715574274765833240, 0.9961946980917454342, 3.870492493070290181E-17 ) ) ;
#10020 = CARTESIAN_POINT ( 'NONE',  ( 0.2819296736111110979, 4.394527777853643791, -3.452642723725051716E-17 ) ) ;
#10021 = CC_DESIGN_DATE_AND_TIME_ASSIGNMENT ( #5380, #3551, ( #7632 ) ) ;
#10022 = ADVANCED_FACE ( 'NONE', ( #19161 ), #9538, .T. ) ;
#10023 = CARTESIAN_POINT ( 'NONE',  ( -0.2078600217396917860, 4.050312593809051620, -0.2327285559015772332 ) ) ;
#10024 = CARTESIAN_POINT ( 'NONE',  ( -0.1144950937579609779, 0.2764156081756484196, 0.02930555555555695163 ) ) ;
#10025 = DIRECTION ( 'NONE',  ( 0.000000000000000000, 0.000000000000000000, 1.000000000000000000 ) ) ;
#10026 = CARTESIAN_POINT ( 'NONE',  ( 0.2819296736111110979, 0.3826388888130222155, 0.000000000000000000 ) ) ;
#10027 = CYLINDRICAL_SURFACE ( 'NONE', #8047, 0.3119999999999999996 ) ;
#10028 = CARTESIAN_POINT ( 'NONE',  ( 2.570936052289255124E-07, 3.738287934957344127, 0.3119999999997750129 ) ) ;
#10029 = CARTESIAN_POINT ( 'NONE',  ( -0.09435543239133792337, 4.111524471938507119, -2.854670964936879329 ) ) ;
#10030 = CARTESIAN_POINT ( 'NONE',  ( -0.2230971623002953874, 0.2230971623002954152, 0.2220138888888916195 ) ) ;
#10031 = ORIENTED_EDGE ( 'NONE', *, *, #21697, .T. ) ;
#10032 = DIRECTION ( 'NONE',  ( -0.8660254037844432595, 0.000000000000000000, 0.4999999999999916733 ) ) ;
#10033 = LINE ( 'NONE', #17455, #6220 ) ;
#10034 = CARTESIAN_POINT ( 'NONE',  ( 0.1993543840281266910, 0.4868055554796889561, -0.1993543840281266910 ) ) ;
#10035 = CARTESIAN_POINT ( 'NONE',  ( 0.1993543840281266355, 0.2506944443685777957, 0.1993543840281267465 ) ) ;
#10036 = CARTESIAN_POINT ( 'NONE',  ( 5.178964085587577574E-17, 4.047305555631421470, 0.2819296736111110979 ) ) ;
#10037 = CARTESIAN_POINT ( 'NONE',  ( -0.2472135954999579999, 0.2232142855192008613, 0.3402603233408159622 ) ) ;
#10038 = CARTESIAN_POINT ( 'NONE',  ( 0.2819296736111110979, 4.557722222298087544, 0.1167790944451422425 ) ) ;
#10039 = CARTESIAN_POINT ( 'NONE',  ( 0.1381111726236976811, 5.088173287601598815, -0.2808105300433598739 ) ) ;
#10040 = ORIENTED_EDGE ( 'NONE', *, *, #15732, .T. ) ;
#10041 = VECTOR ( 'NONE', #1502, 39.37007874015748143 ) ;
#10042 = CARTESIAN_POINT ( 'NONE',  ( -0.3125000000000000000, 1.913510623667739771E-17, 0.2272222222222250176 ) ) ;
#10043 = CARTESIAN_POINT ( 'NONE',  ( 5.731347020009612645E-17, 3.904944444596176734, 0.3119999999999999996 ) ) ;
#10044 = FACE_OUTER_BOUND ( 'NONE', #20387, .T. ) ;
#10045 = EDGE_CURVE ( 'NONE', #6049, #12796, #7586, .T. ) ;
#10046 = CARTESIAN_POINT ( 'NONE',  ( 0.000000000000000000, 5.384999999999999787, 0.000000000000000000 ) ) ;
#10047 = PERSON_AND_ORGANIZATION ( #15518, #2538 ) ;
#10048 = EDGE_CURVE ( 'NONE', #4938, #12247, #16971, .T. ) ;
#10049 = CARTESIAN_POINT ( 'NONE',  ( 0.2716011131362610631, 0.07493431514972453966, 0.3932559629468742601 ) ) ;
#10050 = CARTESIAN_POINT ( 'NONE',  ( -0.2295375298156325794, 5.008762073107971169, 0.2113211636186998754 ) ) ;
#10051 = VERTEX_POINT ( 'NONE', #4644 ) ;
#10052 = CARTESIAN_POINT ( 'NONE',  ( -0.2819296736111110979, 0.02499999992413337591, 0.1167790944451422425 ) ) ;
#10053 = VECTOR ( 'NONE', #5492, 39.37007874015748143 ) ;
#10054 = CARTESIAN_POINT ( 'NONE',  ( 0.2589252677293308325, 4.257452783784655637, -0.1745261803771008813 ) ) ;
#10055 = CARTESIAN_POINT ( 'NONE',  ( 0.1312453311287957169, 0.4543582620183878595, 0.4268234664230710629 ) ) ;
#10056 = CARTESIAN_POINT ( 'NONE',  ( 0.2906323808137692422, 4.082252095162804295, 0.1137463939449124412 ) ) ;
#10057 = CARTESIAN_POINT ( 'NONE',  ( -0.2233192592356399442, 0.3758928570453146656, -0.3073725909049500049 ) ) ;
#10058 = CARTESIAN_POINT ( 'NONE',  ( 0.2912207731228424468, 5.179804787033147839, -0.03491938693372079183 ) ) ;
#10059 = CARTESIAN_POINT ( 'NONE',  ( -0.2923287055106771337, 0.2687499999024575703, 0.2123892367102619971 ) ) ;
#10060 = LINE ( 'NONE', #15658, #4300 ) ;
#10061 = CARTESIAN_POINT ( 'NONE',  ( -0.2819296736111110424, 3.911888888964754507, 0.1167790944451424923 ) ) ;
#10062 = CARTESIAN_POINT ( 'NONE',  ( 0.3040674888080049376, 5.032214460774807385, -0.08102217497193067719 ) ) ;
#10063 = CARTESIAN_POINT ( 'NONE',  ( -0.2322136846690653622, 5.172242893738336456, -0.1834769090104111933 ) ) ;
#10064 = CARTESIAN_POINT ( 'NONE',  ( 0.3950000000000000178, 0.05000000000000028727, -2.591000000000000192 ) ) ;
#10065 = CARTESIAN_POINT ( 'NONE',  ( 0.2206173157302028787, 4.578555555707287894, 0.2206173157302027954 ) ) ;
#10066 = CARTESIAN_POINT ( 'NONE',  ( -0.2819296736111110424, 4.925777777853643791, 0.1167790944451424923 ) ) ;
#10067 = ORIENTED_EDGE ( 'NONE', *, *, #5678, .T. ) ;
#10068 = EDGE_CURVE ( 'NONE', #19497, #21850, #20093, .T. ) ;
#10069 = CARTESIAN_POINT ( 'NONE',  ( -0.1993543840281266910, 3.957027777853642903, -0.1993543840281266910 ) ) ;
#10070 = EDGE_CURVE ( 'NONE', #14874, #21142, #8299, .T. ) ;
#10071 = CONICAL_SURFACE ( 'NONE', #23664, 0.3125000000000000000, 0.7853981633974482790 ) ;
#10072 = EDGE_LOOP ( 'NONE', ( #3997, #21954, #23566, #7276 ) ) ;
#10073 = CARTESIAN_POINT ( 'NONE',  ( -0.3613381517857143788, 0.2473214284738861068, 0.1174058825155740310 ) ) ;
#10074 = VERTEX_POINT ( 'NONE', #21587 ) ;
#10075 = ORIENTED_EDGE ( 'NONE', *, *, #12544, .T. ) ;
#10076 = PERSON_AND_ORGANIZATION ( #15518, #2538 ) ;
#10077 = EDGE_CURVE ( 'NONE', #17585, #7205, #24077, .T. ) ;
#10078 = ORIENTED_EDGE ( 'NONE', *, *, #6162, .T. ) ;
#10079 = DIRECTION ( 'NONE',  ( -1.000000000000000000, 0.000000000000000000, 0.000000000000000000 ) ) ;
#10080 = LINE ( 'NONE', #914, #2659 ) ;
#10081 = CARTESIAN_POINT ( 'NONE',  ( -0.1292346314604058410, 0.1604166665149337478, 0.3119999999999998885 ) ) ;
#10082 = CARTESIAN_POINT ( 'NONE',  ( 0.2408840922389058614, 5.139268827874871270, 0.1879369982435209474 ) ) ;
#10083 = CARTESIAN_POINT ( 'NONE',  ( -0.4687500000000003331, 0.1777514598960921177, 0.4112133685574570485 ) ) ;
#10084 = CARTESIAN_POINT ( 'NONE',  ( -0.2209708691207961095, 0.2209708691207961373, 0.2827777777777814028 ) ) ;
#10085 = CARTESIAN_POINT ( 'NONE',  ( 0.08123675842391495094, 0.06219723018719916507, 0.3013752234401997354 ) ) ;
#10086 = CIRCLE ( 'NONE', #728, 0.1874999999999998335 ) ;
#10087 = CARTESIAN_POINT ( 'NONE',  ( -0.1144950937579609779, 0.2764156081756484196, 0.2445833333333364834 ) ) ;
#10088 = CARTESIAN_POINT ( 'NONE',  ( 0.000000000000000000, 0.9300000000000000488, 0.000000000000000000 ) ) ;
#10089 = CARTESIAN_POINT ( 'NONE',  ( -0.2764156081756484196, -0.1144950937579609362, 0.1473611111111134686 ) ) ;
#10090 = ORIENTED_EDGE ( 'NONE', *, *, #20361, .F. ) ;
#10091 = CARTESIAN_POINT ( 'NONE',  ( 0.1167790944451422702, 4.793833333409199149, -0.2819296736111110424 ) ) ;
#10092 = FACE_OUTER_BOUND ( 'NONE', #23029, .T. ) ;
#10093 = CARTESIAN_POINT ( 'NONE',  ( -1.726321361862525858E-17, 4.672305555631421470, -0.2819296736111110979 ) ) ;
#10094 = CARTESIAN_POINT ( 'NONE',  ( 0.3119999999999998885, 0.2854166665149337478, 0.1292346314604058410 ) ) ;
#10095 = CARTESIAN_POINT ( 'NONE',  ( -0.2503918017774145466, 0.2920750874296680899, -1.186911552162836836 ) ) ;
#10096 = DIRECTION ( 'NONE',  ( 0.000000000000000000, 0.000000000000000000, -1.000000000000000000 ) ) ;
#10097 = CARTESIAN_POINT ( 'NONE',  ( 1.241811370555571286E-09, 4.488277777895108400, -0.3119999999999999996 ) ) ;
#10098 = CARTESIAN_POINT ( 'NONE',  ( -0.2206173157302027676, 4.391055555555555046, 0.2206173157302028787 ) ) ;
#10099 = CARTESIAN_POINT ( 'NONE',  ( 0.2206173157302027954, 5.203555555707287894, -0.2206173157302028232 ) ) ;
#10100 = CARTESIAN_POINT ( 'NONE',  ( 0.3108595454310983386, 4.973660102971597219, 0.02665253488378086996 ) ) ;
#10101 = DIRECTION ( 'NONE',  ( -0.000000000000000000, -1.000000000000000000, -0.000000000000000000 ) ) ;
#10102 = ORIENTED_EDGE ( 'NONE', *, *, #13359, .T. ) ;
#10103 = CARTESIAN_POINT ( 'NONE',  ( 0.000000000000000000, 0.000000000000000000, 1.326383476483184332 ) ) ;
#10104 = ORIENTED_EDGE ( 'NONE', *, *, #18001, .F. ) ;
#10105 = B_SPLINE_CURVE_WITH_KNOTS ( 'NONE', 3,
 ( #23892, #12594, #7210, #16839, #14656, #9277, #3545, #22315, #22077, #5249, #5373, #12720, #18186, #16718, #14782, #6971, #20014, #8424, #22197, #20135, #20258, #8919, #12839, #1956, #3789, #10996, #18424, #5496, #9155, #16600, #5613, #20494, #11235, #3301, #9400, #24020, #7331, #12961 ),
 .UNSPECIFIED., .F., .F.,
 ( 4, 2, 2, 2, 2, 2, 2, 2, 2, 2, 2, 2, 1, 1, 1, 2, 2, 1, 2, 2, 4 ),
 ( 0.5573884401815307754, 0.5596720767556532250, 0.5608138950427145053, 0.5619557133297757856, 0.5630975316168369549, 0.5642393499038982352, 0.5653811681909595155, 0.5665229864780206848, 0.5676648047650819651, 0.5688066230521432454, 0.5693775321956737745, 0.5696629867674390946, 0.5698057140533218101, 0.5698770776962630569, 0.5699127595177337913, 0.5699306004284691030, 0.5699395208838368143, 0.5699484413392044146, 0.5710902596262658060, 0.5733738962003884776, 0.5756575327745111492 ),
 .UNSPECIFIED. ) ;
#10106 = DIRECTION ( 'NONE',  ( -2.489328460184014472E-15, -0.9607689228305229534, 0.2773500981126141296 ) ) ;
#10107 = AXIS2_PLACEMENT_3D ( 'NONE', #21293, #20036, #4586 ) ;
#10108 = ORIENTED_EDGE ( 'NONE', *, *, #10876, .F. ) ;
#10109 = CARTESIAN_POINT ( 'NONE',  ( 0.1240224521522770712, 4.130797334433546908, 0.2867944741873222347 ) ) ;
#10110 = CARTESIAN_POINT ( 'NONE',  ( -0.2230971623002954152, -0.2230971623002953874, 0.1282638888888912865 ) ) ;
#10111 = CARTESIAN_POINT ( 'NONE',  ( -0.3101174172661915196, -0.3622195030262472804, 0.08858683671056802322 ) ) ;
#10112 = CARTESIAN_POINT ( 'NONE',  ( -0.3613381517857143232, -0.04553571438325666049, -0.1174058825155741004 ) ) ;
#10113 = CARTESIAN_POINT ( 'NONE',  ( -0.04827834974809647184, 0.03398119426037959911, 0.2819296736111110979 ) ) ;
#10114 = CARTESIAN_POINT ( 'NONE',  ( 0.2764156081756483641, -0.1144950937579611167, -0.1026388888888885437 ) ) ;
#10115 = CARTESIAN_POINT ( 'NONE',  ( 0.000000000000000000, 3.659999999999999698, 0.000000000000000000 ) ) ;
#10116 = CARTESIAN_POINT ( 'NONE',  ( 2.911000000000000032, 2.689999999999999947, 0.000000000000000000 ) ) ;
#10117 = CARTESIAN_POINT ( 'NONE',  ( 0.1144950937579609085, -0.2764156081756484751, 0.3904166666666708529 ) ) ;
#10118 = ORIENTED_EDGE ( 'NONE', *, *, #5151, .F. ) ;
#10119 = FACE_OUTER_BOUND ( 'NONE', #4418, .T. ) ;
#10120 = DIRECTION ( 'NONE',  ( -0.000000000000000000, -1.000000000000000000, -0.000000000000000000 ) ) ;
#10121 = DIRECTION ( 'NONE',  ( 0.000000000000000000, -0.000000000000000000, 1.000000000000000000 ) ) ;
#10122 = CARTESIAN_POINT ( 'NONE',  ( -0.1292346314604058410, 0.5006944444444441089, 0.3119999999999998885 ) ) ;
#10123 = CARTESIAN_POINT ( 'NONE',  ( -0.3119999999999999996, 4.880638888888888083, -0.1292346314604056468 ) ) ;
#10124 = AXIS2_PLACEMENT_3D ( 'NONE', #21453, #23262, #19617 ) ;
#10125 = CARTESIAN_POINT ( 'NONE',  ( -0.2819296736111110424, 3.974388888964754507, -0.1167790944451423119 ) ) ;
#10126 = DIRECTION ( 'NONE',  ( 0.000000000000000000, -0.000000000000000000, -1.000000000000000000 ) ) ;
#10127 = CARTESIAN_POINT ( 'NONE',  ( 0.1797085267211815662, 3.721720965436318362, -0.2172307213220433242 ) ) ;
#10128 = CARTESIAN_POINT ( 'NONE',  ( 0.2405467123332261370, 4.813840729788613437, -0.2030146156137226099 ) ) ;
#10129 = EDGE_LOOP ( 'NONE', ( #4502, #5260, #13893, #10245, #21512, #13249 ) ) ;
#10130 = VERTEX_POINT ( 'NONE', #4527 ) ;
#10131 = DIRECTION ( 'NONE',  ( 0.4472135954999560403, -0.4472135954999560403, 0.7745966692414856247 ) ) ;
#10132 = CARTESIAN_POINT ( 'NONE',  ( 0.2819296736111110424, 4.828555555631420582, -0.1167790944451423396 ) ) ;
#10133 = CARTESIAN_POINT ( 'NONE',  ( 0.1653103785569666750, -0.4584405057248004955, 0.07159583130656670125 ) ) ;
#10134 = CARTESIAN_POINT ( 'NONE',  ( 5.731347020009612645E-17, 4.120222222222221120, 0.3119999999999999996 ) ) ;
#10135 = ADVANCED_FACE ( 'NONE', ( #15751 ), #748, .F. ) ;
#10136 =( NAMED_UNIT ( * ) SI_UNIT ( $, .STERADIAN. ) SOLID_ANGLE_UNIT ( ) );
#10137 = FACE_OUTER_BOUND ( 'NONE', #10565, .T. ) ;
#10138 = VECTOR ( 'NONE', #15062, 39.37007874015748143 ) ;
#10139 = CARTESIAN_POINT ( 'NONE',  ( -0.1954553509668046918, -0.1954553509668046640, 0.03972222222222369925 ) ) ;
#10140 = VECTOR ( 'NONE', #17099, 39.37007874015748854 ) ;
#10141 = CARTESIAN_POINT ( 'NONE',  ( 0.1993543840281266633, 4.290361111186976828, -0.1993543840281266910 ) ) ;
#10142 = FACE_OUTER_BOUND ( 'NONE', #23662, .T. ) ;
#10143 = LINE ( 'NONE', #17567, #4673 ) ;
#10144 = CARTESIAN_POINT ( 'NONE',  ( 0.2764156081756483641, 0.1144950937579610195, 0.1265277777777799595 ) ) ;
#10145 = CARTESIAN_POINT ( 'NONE',  ( 9.101228903679513089E-16, 0.2392857142857141850, 0.4000000000000000222 ) ) ;
#10146 = CARTESIAN_POINT ( 'NONE',  ( -0.2819296736111110979, 0.4104166665908000056, -3.452642723725051716E-17 ) ) ;
#10147 = CARTESIAN_POINT ( 'NONE',  ( -0.1292346314604058410, 0.1118055555555552139, 0.3119999999999998885 ) ) ;
#10148 = CARTESIAN_POINT ( 'NONE',  ( 5.731347020009612645E-17, 4.453555555555555046, 0.3119999999999999996 ) ) ;
#10149 = CARTESIAN_POINT ( 'NONE',  ( 0.4000000000000000222, 0.3285714285714284588, 0.000000000000000000 ) ) ;
#10150 = CARTESIAN_POINT ( 'NONE',  ( -3.863846776457871776E-17, -0.3155070326520292845, 0.4650694444444490872 ) ) ;
#10151 = CARTESIAN_POINT ( 'NONE',  ( -0.1294417382415922191, 0.3125000000000000000, 0.05013888888889027340 ) ) ;
#10152 = CARTESIAN_POINT ( 'NONE',  ( -0.04072772395942860640, 3.767161843808154664, -0.3094987719763222511 ) ) ;
#10153 = CARTESIAN_POINT ( 'NONE',  ( -0.1167790944451424506, 0.5736111110352444253, 0.2819296736111110424 ) ) ;
#10154 = CARTESIAN_POINT ( 'NONE',  ( -0.1993543840281266633, 0.4451388888130222710, -0.1993543840281266910 ) ) ;
#10155 = CARTESIAN_POINT ( 'NONE',  ( 5.178964085587577574E-17, 4.102861111186976828, 0.2819296736111110979 ) ) ;
#10156 = CARTESIAN_POINT ( 'NONE',  ( -0.2472135954999579444, 0.2732142855192009057, -0.3402603233408159622 ) ) ;
#10157 = CARTESIAN_POINT ( 'NONE',  ( -0.1993543840281266355, 4.595916666742532186, 0.1993543840281267465 ) ) ;
#10158 = CARTESIAN_POINT ( 'NONE',  ( 0.3850708708653794998, -0.3189451064140639280, 0.07813342133392808808 ) ) ;
#10159 = VECTOR ( 'NONE', #8506, 39.37007874015748854 ) ;
#10160 = CARTESIAN_POINT ( 'NONE',  ( 0.1236067977499789028, 0.1624999998049151961, 0.3804226065180614791 ) ) ;
#10161 = AXIS2_PLACEMENT_3D ( 'NONE', #4993, #5358, #12457 ) ;
#10162 = VERTEX_POINT ( 'NONE', #12676 ) ;
#10163 = CARTESIAN_POINT ( 'NONE',  ( -1.910449006669871087E-17, 4.036888888888888083, -0.3119999999999999996 ) ) ;
#10164 = CARTESIAN_POINT ( 'NONE',  ( 0.1292346314604058410, 3.797305555707287894, 0.3119999999999998885 ) ) ;
#10165 = APPROVAL ( #22265, 'UNSPECIFIED' ) ;
#10166 = CARTESIAN_POINT ( 'NONE',  ( 1.397631139260601341, 2.978485840173427324, -2.174029041877829638 ) ) ;
#10167 = VERTEX_POINT ( 'NONE', #19280 ) ;
#10168 = COORDINATED_UNIVERSAL_TIME_OFFSET ( 0, 0, .AHEAD. ) ;
#10169 = ORIENTED_EDGE ( 'NONE', *, *, #1590, .T. ) ;
#10170 = CARTESIAN_POINT ( 'NONE',  ( 0.4000000000000000222, 0.3285714285714284588, 0.000000000000000000 ) ) ;
#10171 = VECTOR ( 'NONE', #6316, 39.37007874015748143 ) ;
#10172 = FACE_OUTER_BOUND ( 'NONE', #23891, .T. ) ;
#10173 = VERTEX_POINT ( 'NONE', #13926 ) ;
#10174 = CARTESIAN_POINT ( 'NONE',  ( 0.1167790944451423535, 0.03888888881302225708, 0.2819296736111110424 ) ) ;
#10175 = AXIS2_PLACEMENT_3D ( 'NONE', #3392, #1449, #12439 ) ;
#10176 = ORIENTED_EDGE ( 'NONE', *, *, #17163, .F. ) ;
#10177 = CARTESIAN_POINT ( 'NONE',  ( 0.2872988799765124335, 4.255711475989661707, -0.1216958920792224202 ) ) ;
#10178 = CARTESIAN_POINT ( 'NONE',  ( -0.3069366055884749644, 4.722600365735013739, -0.06133714766361197945 ) ) ;
#10179 = CARTESIAN_POINT ( 'NONE',  ( 0.3002986933836771510, 4.083101498185607525, 0.08467756203784890245 ) ) ;
#10180 = CARTESIAN_POINT ( 'NONE',  ( 0.3613381517857143232, 0.3473214284738860291, 0.1174058825155742114 ) ) ;
#10181 = CARTESIAN_POINT ( 'NONE',  ( 0.2005216093553227330, 5.172899910562626324, 0.2173648676198124963 ) ) ;
#10182 = CARTESIAN_POINT ( 'NONE',  ( 0.2923287055106771337, 0.4330357141881717720, 0.2123892367102621359 ) ) ;
#10183 = DIRECTION ( 'NONE',  ( 0.08715574274765830465, -0.9961946980917454342, -3.870492493070289564E-17 ) ) ;
#10184 = CARTESIAN_POINT ( 'NONE',  ( -0.1167790944451423257, 3.842444444520309865, -0.2819296736111110424 ) ) ;
#10185 = CARTESIAN_POINT ( 'NONE',  ( 0.3035936216127623211, 5.027565645647625203, 0.08278009126895921610 ) ) ;
#10186 = DIRECTION ( 'NONE',  ( 0.000000000000000000, 0.000000000000000000, 1.000000000000000000 ) ) ;
#10187 = DIRECTION ( 'NONE',  ( 0.000000000000000000, 0.000000000000000000, -1.000000000000000000 ) ) ;
#10188 = CARTESIAN_POINT ( 'NONE',  ( 0.3119999999999999996, 4.585500000151731648, -3.820898013339742174E-17 ) ) ;
#10189 = EDGE_CURVE ( 'NONE', #19562, #15412, #3393, .T. ) ;
#10190 = CARTESIAN_POINT ( 'NONE',  ( -0.1167790944451423119, 4.634111111186976828, -0.2819296736111110979 ) ) ;
#10191 = VERTEX_POINT ( 'NONE', #21113 ) ;
#10192 = CARTESIAN_POINT ( 'NONE',  ( 0.1167790944451422702, 4.113277777853642903, -0.2819296736111110424 ) ) ;
#10193 = ORIENTED_EDGE ( 'NONE', *, *, #9313, .F. ) ;
#10194 = VERTEX_POINT ( 'NONE', #4403 ) ;
#10195 = CALENDAR_DATE ( 2026, 7, 10 ) ;
#10196 = ORIENTED_EDGE ( 'NONE', *, *, #17114, .F. ) ;
#10197 = FACE_OUTER_BOUND ( 'NONE', #17543, .T. ) ;
#10198 = CARTESIAN_POINT ( 'NONE',  ( -6.389700406101856968E-07, 4.404919069638722817, 0.3119999999986028949 ) ) ;
#10199 = ORIENTED_EDGE ( 'NONE', *, *, #10667, .T. ) ;
#10200 = CARTESIAN_POINT ( 'NONE',  ( -0.1292346314604058410, 0.1048611109593781815, 0.3119999999999998885 ) ) ;
#10201 = FACE_OUTER_BOUND ( 'NONE', #112, .T. ) ;
#10202 = CARTESIAN_POINT ( 'NONE',  ( -0.4581189881604794678, 0.2644951211353315235, 0.3941886329748526263 ) ) ;
#10203 = CARTESIAN_POINT ( 'NONE',  ( 5.731347020009612645E-17, 4.453555555555555046, 0.3119999999999999996 ) ) ;
#10204 = EDGE_CURVE ( 'NONE', #10793, #23698, #10033, .T. ) ;
#10205 = DIRECTION ( 'NONE',  ( -0.08715574274765827689, 0.9961946980917454342, -5.815890212748468633E-18 ) ) ;
#10206 = CARTESIAN_POINT ( 'NONE',  ( 0.1993543840281266355, 0.1395833332574667185, 0.1993543840281267465 ) ) ;
#10207 = CARTESIAN_POINT ( 'NONE',  ( 0.1144950937579609085, -0.2764156081756484751, 0.1612500000000025024 ) ) ;
#10208 = DIRECTION ( 'NONE',  ( 0.000000000000000000, 0.000000000000000000, 1.000000000000000000 ) ) ;
#10209 = CARTESIAN_POINT ( 'NONE',  ( 0.1167790944451424368, 4.370222222298088433, 0.2819296736111110424 ) ) ;
#10210 = CARTESIAN_POINT ( 'NONE',  ( 0.2951834061891078775, 0.03795937687255809129, -0.08618158780276162501 ) ) ;
#10211 = DIRECTION ( 'NONE',  ( 0.000000000000000000, -0.9607689228305228424, -0.2773500981126148512 ) ) ;
#10212 = FACE_OUTER_BOUND ( 'NONE', #21539, .T. ) ;
#10213 = CARTESIAN_POINT ( 'NONE',  ( 0.2206173157302027676, 0.4486111109593781676, 0.2206173157302028787 ) ) ;
#10214 = CARTESIAN_POINT ( 'NONE',  ( -0.3119999999999999996, 4.213972222222222008, -0.1292346314604056468 ) ) ;
#10215 = CARTESIAN_POINT ( 'NONE',  ( 0.000000000000000000, 5.580000000000000959, 0.000000000000000000 ) ) ;
#10216 = CARTESIAN_POINT ( 'NONE',  ( 0.1292346314604058410, 5.068138888888888083, 0.3119999999999998885 ) ) ;
#10217 = EDGE_CURVE ( 'NONE', #1943, #18699, #13482, .T. ) ;
#10218 = CARTESIAN_POINT ( 'NONE',  ( 0.2635330294133203521, 4.979450665808103693, -0.1720186351255787172 ) ) ;
#10219 = CARTESIAN_POINT ( 'NONE',  ( 0.1586475693114279273, 0.4496706605170417981, 0.08858850926231193190 ) ) ;
#10220 = ORIENTED_EDGE ( 'NONE', *, *, #21071, .F. ) ;
#10221 = CARTESIAN_POINT ( 'NONE',  ( -0.1294417382415922746, -0.3125000000000000000, 0.07791666666666866026 ) ) ;
#10222 = CARTESIAN_POINT ( 'NONE',  ( 0.3127913692903316334, 4.140747938380851423, 0.009870907807890409030 ) ) ;
#10223 = CARTESIAN_POINT ( 'NONE',  ( -0.1306872919485615459, -0.3155070326520293400, -0.03493055555555446556 ) ) ;
#10224 = VECTOR ( 'NONE', #15216, 39.37007874015748143 ) ;
#10225 = DIRECTION ( 'NONE',  ( -1.000000000000000000, 0.000000000000000000, 0.000000000000000000 ) ) ;
#10226 = CARTESIAN_POINT ( 'NONE',  ( 0.2923287055106771337, 0.1294642856167433076, 0.2123892367102621359 ) ) ;
#10227 = ADVANCED_FACE ( 'NONE', ( #13601 ), #9687, .T. ) ;
#10228 = CARTESIAN_POINT ( 'NONE',  ( 1.573500000000000343, 0.000000000000000000, -0.5399999999999998135 ) ) ;
#10229 = CARTESIAN_POINT ( 'NONE',  ( -0.2764156081756484196, 0.1144950937579609918, -0.07486111111111054539 ) ) ;
#10230 = DIRECTION ( 'NONE',  ( 0.000000000000000000, 0.000000000000000000, -1.000000000000000000 ) ) ;
#10231 = CARTESIAN_POINT ( 'NONE',  ( 0.4687500000000002776, 0.2706329386826373806, 0.4425000000000000044 ) ) ;
#10232 = CARTESIAN_POINT ( 'NONE',  ( 0.1954553509668047195, 0.1954553509668046085, 0.4077777777777821799 ) ) ;
#10233 = ORIENTED_EDGE ( 'NONE', *, *, #10624, .F. ) ;
#10234 = CARTESIAN_POINT ( 'NONE',  ( 6.388359114324787822E-07, 4.627192232271967853, 0.3119999999985919592 ) ) ;
#10235 = FACE_OUTER_BOUND ( 'NONE', #4211, .T. ) ;
#10236 = DIRECTION ( 'NONE',  ( 0.000000000000000000, -1.000000000000000000, 0.000000000000000000 ) ) ;
#10237 = CARTESIAN_POINT ( 'NONE',  ( -0.2206173157302027954, 0.3722222222222218990, -0.2206173157302028232 ) ) ;
#10238 = CARTESIAN_POINT ( 'NONE',  ( -0.3119999999999999996, 4.936194444444443441, -0.1292346314604056468 ) ) ;
#10239 = CARTESIAN_POINT ( 'NONE',  ( 0.1167790944451424506, 4.148000000075866112, 0.2819296736111110424 ) ) ;
#10240 = CARTESIAN_POINT ( 'NONE',  ( -0.1993543840281266910, 3.970916666742532186, -0.1993543840281266910 ) ) ;
#10241 = EDGE_CURVE ( 'NONE', #5752, #2198, #10566, .T. ) ;
#10242 = CARTESIAN_POINT ( 'NONE',  ( 0.000000000000000000, 2.291712385858714729, 0.03922008423644621905 ) ) ;
#10243 = DIRECTION ( 'NONE',  ( 0.08715574274765830465, -0.9961946980917454342, -3.870492493070289564E-17 ) ) ;
#10244 = CARTESIAN_POINT ( 'NONE',  ( 0.3125925260372354741, 4.808137523523458690, -0.01455662600646890834 ) ) ;
#10245 = ORIENTED_EDGE ( 'NONE', *, *, #3372, .T. ) ;
#10246 = ORIENTED_EDGE ( 'NONE', *, *, #17834, .T. ) ;
#10247 = CARTESIAN_POINT ( 'NONE',  ( 0.1294417382415921358, -0.3125000000000002220, -0.02624999999999886105 ) ) ;
#10248 = CARTESIAN_POINT ( 'NONE',  ( 0.1167790944451424368, 4.759111111186977716, 0.2819296736111110424 ) ) ;
#10249 = VECTOR ( 'NONE', #22195, 39.37007874015748143 ) ;
#10250 = FACE_OUTER_BOUND ( 'NONE', #16209, .T. ) ;
#10251 = CARTESIAN_POINT ( 'NONE',  ( -0.007894445728632182302, 4.515849982952590658, 0.3119999997756114363 ) ) ;
#10252 = PERSON_AND_ORGANIZATION ( #15518, #2538 ) ;
#10253 = CARTESIAN_POINT ( 'NONE',  ( -0.4802534441549711763, -0.2139678024937353706, 0.05347141629229230919 ) ) ;
#10254 = CARTESIAN_POINT ( 'NONE',  ( -0.1144950937579609779, 0.2764156081756484196, -0.08874999999999953759 ) ) ;
#10255 = CARTESIAN_POINT ( 'NONE',  ( 0.2819296736111110979, 4.064666666742532186, -0.1167790944451423396 ) ) ;
#10256 = DATE_AND_TIME ( #21223, #16217 ) ;
#10257 = DIRECTION ( 'NONE',  ( 0.000000000000000000, 0.000000000000000000, 1.000000000000000000 ) ) ;
#10258 = FACE_OUTER_BOUND ( 'NONE', #18590, .T. ) ;
#10259 = CARTESIAN_POINT ( 'NONE',  ( 0.1144950937579611444, 0.2764156081756483641, 0.1890277777777804313 ) ) ;
#10260 = CARTESIAN_POINT ( 'NONE',  ( 0.2472135954999579721, 0.2678571428571427382, -0.3402603233408160732 ) ) ;
#10261 = CARTESIAN_POINT ( 'NONE',  ( -0.2819296736111110424, 0.1152777777019111521, -0.1167790944451423396 ) ) ;
#10262 = CARTESIAN_POINT ( 'NONE',  ( 0.4687500000000002776, -0.04414274412020515598, 0.09139217954989621584 ) ) ;
#10263 = CARTESIAN_POINT ( 'NONE',  ( 0.000000000000000000, 5.384999999999999787, -0.3119999999999999996 ) ) ;
#10264 = FACE_OUTER_BOUND ( 'NONE', #17497, .T. ) ;
#10265 = CARTESIAN_POINT ( 'NONE',  ( -1.493307031895086562E-17, 0.6673231647285333690, -1.029600057125203305 ) ) ;
#10266 = CARTESIAN_POINT ( 'NONE',  ( 0.3155070326520292290, -0.1306872919485616569, 0.3643750000000038902 ) ) ;
#10267 = AXIS2_PLACEMENT_3D ( 'NONE', #1381, #6742, #12739 ) ;
#10268 = VERTEX_POINT ( 'NONE', #15297 ) ;
#10269 = CARTESIAN_POINT ( 'NONE',  ( 0.4593750000000003664, 0.2760455974562901482, 0.06112444011295366936 ) ) ;
#10270 = CARTESIAN_POINT ( 'NONE',  ( 2.986000000000000210, 2.690000000000002167, 0.000000000000000000 ) ) ;
#10271 = CARTESIAN_POINT ( 'NONE',  ( -0.3125000000000000000, 1.913510623667739771E-17, 0.005000000000001014917 ) ) ;
#10272 = CARTESIAN_POINT ( 'NONE',  ( -0.2819296736111110979, 0.3409722221463556413, -3.452642723725051716E-17 ) ) ;
#10273 = CARTESIAN_POINT ( 'NONE',  ( -1.726321361862525858E-17, 4.075083333409199149, -0.2819296736111110979 ) ) ;
#10274 = CARTESIAN_POINT ( 'NONE',  ( -0.4000000000000000222, 0.4267857140906294866, -4.898587196589413075E-17 ) ) ;
#10275 = ADVANCED_FACE ( 'NONE', ( #22359 ), #3112, .F. ) ;
#10276 = EDGE_LOOP ( 'NONE', ( #17889, #6665, #11698, #9734 ) ) ;
#10277 = CARTESIAN_POINT ( 'NONE',  ( -0.1993543840281266910, 4.693138888964754507, -0.1993543840281266910 ) ) ;
#10278 = ADVANCED_FACE ( 'NONE', ( #654 ), #9565, .T. ) ;
#10279 = DIRECTION ( 'NONE',  ( -0.8660254037844438146, 0.000000000000000000, -0.4999999999999911737 ) ) ;
#10280 = CARTESIAN_POINT ( 'NONE',  ( 0.2883059669956098969, 5.075061251213828228, 0.1201015347656402971 ) ) ;
#10281 = ORIENTED_EDGE ( 'NONE', *, *, #8677, .F. ) ;
#10282 = DIRECTION ( 'NONE',  ( 0.7071067811865514585, -0.7071067811865436870, 0.000000000000000000 ) ) ;
#10283 = CARTESIAN_POINT ( 'NONE',  ( -0.3119999999999999996, 3.891055555707287894, 0.000000000000000000 ) ) ;
#10284 = DIRECTION ( 'NONE',  ( 0.000000000000000000, 1.000000000000000000, 0.000000000000000000 ) ) ;
#10285 = DIRECTION ( 'NONE',  ( 0.000000000000000000, 0.000000000000000000, -1.000000000000000000 ) ) ;
#10286 = CARTESIAN_POINT ( 'NONE',  ( 0.1629873018068623836, 5.206640035683670398, 0.2306973944900186091 ) ) ;
#10287 = CARTESIAN_POINT ( 'NONE',  ( 0.1993543840281266633, 4.998694444520309865, -0.1993543840281266910 ) ) ;
#10288 = DATE_AND_TIME ( #763, #17367 ) ;
#10289 = ORIENTED_EDGE ( 'NONE', *, *, #14848, .F. ) ;
#10290 = CARTESIAN_POINT ( 'NONE',  ( -0.3086545942380659047, 5.114261002539869594, -0.02184028893379939135 ) ) ;
#10291 = CARTESIAN_POINT ( 'NONE',  ( 0.3119999999999999996, 0.2437499999999996891, -0.1292346314604056468 ) ) ;
#10292 = ORIENTED_EDGE ( 'NONE', *, *, #10822, .F. ) ;
#10293 = CARTESIAN_POINT ( 'NONE',  ( -5.178964085587577574E-17, 0.03541666659080003332, 0.2819296736111110979 ) ) ;
#10294 = VERTEX_POINT ( 'NONE', #13127 ) ;
#10295 = CARTESIAN_POINT ( 'NONE',  ( 0.1167790944451423257, 0.004166666590800035055, -0.2819296736111110424 ) ) ;
#10296 = CYLINDRICAL_SURFACE ( 'NONE', #16223, 0.3125000000000000000 ) ;
#10297 = CARTESIAN_POINT ( 'NONE',  ( 0.2985525202959439239, 4.082927124627439674, 0.09073774551547199307 ) ) ;
#10298 = CARTESIAN_POINT ( 'NONE',  ( 0.3613381517857143232, 0.2080357141881718774, 0.000000000000000000 ) ) ;
#10299 = CARTESIAN_POINT ( 'NONE',  ( -0.2925124024682271284, 5.054586912992379943, -0.1086053545779250423 ) ) ;
#10300 = PERSON ( 'NAUO-PER4', 'UNSPECIFIED', 'UNSPECIFIED', ('UNSPECIFIED'), ('UNSPECIFIED'), ('UNSPECIFIED') ) ;
#10301 = CARTESIAN_POINT ( 'NONE',  ( 0.000000000000000000, 0.4202679491924311561, 0.000000000000000000 ) ) ;
#10302 = CARTESIAN_POINT ( 'NONE',  ( -0.2722828206202175805, 4.664154358537332179, -0.1577052281583355975 ) ) ;
#10303 = AXIS2_PLACEMENT_3D ( 'NONE', #21912, #12551, #18264 ) ;
#10304 = CARTESIAN_POINT ( 'NONE',  ( 0.2819296736111110424, 3.773000000075866112, -0.1167790944451423396 ) ) ;
#10305 = CARTESIAN_POINT ( 'NONE',  ( 0.05068837741648516554, 5.073009555618063438, 0.3078549794868774558 ) ) ;
#10306 = CARTESIAN_POINT ( 'NONE',  ( 1.573500000000000343, -3.414809992080329023E-17, -1.875000000000000000 ) ) ;
#10307 = CARTESIAN_POINT ( 'NONE',  ( 0.3119999999999999996, 4.533416666818399499, -0.1292346314604056745 ) ) ;
#10308 = CARTESIAN_POINT ( 'NONE',  ( 0.1167790944451424506, 4.828555555631421470, 0.2819296736111110424 ) ) ;
#10309 = ORIENTED_EDGE ( 'NONE', *, *, #3946, .T. ) ;
#10310 = AXIS2_PLACEMENT_3D ( 'NONE', #17080, #22565, #5856 ) ;
#10311 = EDGE_CURVE ( 'NONE', #11169, #15529, #10937, .T. ) ;
#10312 = CARTESIAN_POINT ( 'NONE',  ( -0.2819296736111110424, 4.023000000075866112, 0.1167790944451424923 ) ) ;
#10313 = ORIENTED_EDGE ( 'NONE', *, *, #10701, .T. ) ;
#10314 = DATE_TIME_ROLE ( 'classification_date' ) ;
#10315 = AXIS2_PLACEMENT_3D ( 'NONE', #1387, #23438, #14193 ) ;
#10316 = ORIENTED_EDGE ( 'NONE', *, *, #4658, .F. ) ;
#10317 = DIRECTION ( 'NONE',  ( 0.000000000000000000, 0.000000000000000000, -1.000000000000000000 ) ) ;
#10318 = DIRECTION ( 'NONE',  ( 0.000000000000000000, -0.000000000000000000, 1.000000000000000000 ) ) ;
#10319 = CARTESIAN_POINT ( 'NONE',  ( -0.2206173157302027954, 0.1430555554038226151, -0.2206173157302028232 ) ) ;
#10321 = CARTESIAN_POINT ( 'NONE',  ( 0.2995508976399182122, 5.147601669199691976, -0.04633967184963520836 ) ) ;
#10320 = B_SPLINE_CURVE_WITH_KNOTS ( 'NONE', 3,
 ( #9239, #2043, #16914, #20697, #8997, #14743, #16440, #12798, #22037, #5333, #20217, #10957, #18382, #1677, #9110, #16560, #23981, #13750, #11681, #8003, #8116, #13637, #15570, #4229, #9972, #22993, #21174, #4464, #18992, #15334, #13520 ),
 .UNSPECIFIED., .F., .F.,
 ( 4, 2, 2, 2, 2, 2, 2, 2, 2, 2, 2, 1, 1, 1, 1, 1, 2, 4 ),
 ( 0.6853182142057806514, 0.6864601233937474012, 0.6876020325817142620, 0.6898858509576478726, 0.6921696693335813722, 0.6944534877095149827, 0.6967373060854485933, 0.6990211244613822039, 0.7013049428373157035, 0.7024468520252825643, 0.7030178066192659392, 0.7033032839162576266, 0.7034460225647534148, 0.7035173918890014200, 0.7035530765511253115, 0.7035709188821873683, 0.7035798400477183412, 0.7035887612132493141 ),
 .UNSPECIFIED. ) ;
#10322 = CC_DESIGN_DATE_AND_TIME_ASSIGNMENT ( #19036, #20739, ( #6483 ) ) ;
#10323 = CARTESIAN_POINT ( 'NONE',  ( -0.4687500000000003886, -0.1778076022956336377, 0.4111980179219333342 ) ) ;
#10324 = CARTESIAN_POINT ( 'NONE',  ( 0.01406054063584270125, 0.1559579195750173675, -0.7499011851857120270 ) ) ;
#10325 = CARTESIAN_POINT ( 'NONE',  ( 0.000000000000000000, 5.384999999999999787, 0.000000000000000000 ) ) ;
#10326 = CARTESIAN_POINT ( 'NONE',  ( -0.1167790944451422702, 0.05277777770191114520, -0.2819296736111110979 ) ) ;
#10327 = CARTESIAN_POINT ( 'NONE',  ( 0.2764156081756484196, -5.077672346800151106E-17, 0.06055555555555720143 ) ) ;
#10328 = FACE_OUTER_BOUND ( 'NONE', #6439, .T. ) ;
#10329 = CARTESIAN_POINT ( 'NONE',  ( 0.1993543840281267465, 4.429250000075865223, 0.1993543840281266633 ) ) ;
#10330 = CARTESIAN_POINT ( 'NONE',  ( -0.08610082984204266154, 0.2741627315343084792, -0.07637567569807812706 ) ) ;
#10331 = CARTESIAN_POINT ( 'NONE',  ( -0.2371368682194363309, 0.2772055556030146861, -1.193725331483267205 ) ) ;
#10332 = FACE_OUTER_BOUND ( 'NONE', #2325, .T. ) ;
#10333 = LINE ( 'NONE', #4946, #11602 ) ;
#10334 = CARTESIAN_POINT ( 'NONE',  ( -0.3119999999999999996, 4.380638888888888083, -0.1292346314604056468 ) ) ;
#10335 = CARTESIAN_POINT ( 'NONE',  ( 0.3119999999999999996, 5.137583333485064685, 0.1292346314604056190 ) ) ;
#10336 = AXIS2_PLACEMENT_3D ( 'NONE', #21929, #5224, #12695 ) ;
#10337 = CARTESIAN_POINT ( 'NONE',  ( -0.1292346314604044810, 4.672305555555555934, 0.3120000000000012208 ) ) ;
#10338 = CARTESIAN_POINT ( 'NONE',  ( 0.2723952011404801032, 0.3839984346608560917, 0.09139143879391152525 ) ) ;
#10339 = VERTEX_POINT ( 'NONE', #20658 ) ;
#10340 = CC_DESIGN_APPROVAL ( #18042, ( #14477 ) ) ;
#10341 = DIRECTION ( 'NONE',  ( -0.000000000000000000, 1.000000000000000000, -0.000000000000000000 ) ) ;
#10342 = EDGE_CURVE ( 'NONE', #16571, #4057, #18214, .T. ) ;
#10343 = CARTESIAN_POINT ( 'NONE',  ( 0.4687500000000003886, -0.2570931668155774785, 0.04874733047934001057 ) ) ;
#10344 = CARTESIAN_POINT ( 'NONE',  ( -0.3155070326520293400, -0.1306872919485614626, -0.04187499999999895473 ) ) ;
#10345 = DIRECTION ( 'NONE',  ( 1.000000000000000000, 0.000000000000000000, 0.000000000000000000 ) ) ;
#10346 = CIRCLE ( 'NONE', #16574, 0.01875000000000000278 ) ;
#10347 = DIRECTION ( 'NONE',  ( 0.000000000000000000, 0.000000000000000000, -1.000000000000000000 ) ) ;
#10348 = ADVANCED_FACE ( 'NONE', ( #5781 ), #23193, .F. ) ;
#10349 = VERTEX_POINT ( 'NONE', #19427 ) ;
#10350 = CARTESIAN_POINT ( 'NONE',  ( -0.2233192592356399997, 0.3258928570453145657, 0.3073725909049499494 ) ) ;
#10351 = CARTESIAN_POINT ( 'NONE',  ( 0.1993543840281266910, 0.1118055554796889145, -0.1993543840281266910 ) ) ;
#10352 = CARTESIAN_POINT ( 'NONE',  ( -0.1144950937579609918, -0.2764156081756484196, -0.005416666666665557496 ) ) ;
#10353 = CARTESIAN_POINT ( 'NONE',  ( -1.184579095217545452, 4.111524471938507119, -2.252250032325342488 ) ) ;
#10354 = CARTESIAN_POINT ( 'NONE',  ( -0.3050515993604162590, -0.01759458571372108510, -0.09459994310003677631 ) ) ;
#10355 = CARTESIAN_POINT ( 'NONE',  ( 0.1954553509668047195, 0.1954553509668046085, 0.4633333333333381487 ) ) ;
#10356 = ORIENTED_EDGE ( 'NONE', *, *, #16892, .F. ) ;
#10357 = FACE_OUTER_BOUND ( 'NONE', #699, .T. ) ;
#10358 = CARTESIAN_POINT ( 'NONE',  ( -0.09248661545808961604, 4.268693300206678032, -0.2987603559195510794 ) ) ;
#10359 = CC_DESIGN_APPROVAL ( #22804, ( #2989 ) ) ;
#10360 = CARTESIAN_POINT ( 'NONE',  ( 0.000000000000000000, 0.000000000000000000, 0.000000000000000000 ) ) ;
#10361 = CARTESIAN_POINT ( 'NONE',  ( 0.3119999999999999996, 0.4069444444444440534, 0.000000000000000000 ) ) ;
#10362 = CARTESIAN_POINT ( 'NONE',  ( 0.2206173157302027954, 4.918833333333332725, -0.2206173157302028232 ) ) ;
#10363 = CARTESIAN_POINT ( 'NONE',  ( 0.2819296736111110979, 4.158416666742532186, -3.452642723725051716E-17 ) ) ;
#10364 = CARTESIAN_POINT ( 'NONE',  ( 0.2819296736111110979, 3.946611111186976384, 0.1167790944451422425 ) ) ;
#10365 = PLANE ( 'NONE',  #23265 ) ;
#10366 = CARTESIAN_POINT ( 'NONE',  ( 0.3108998888495465018, 4.807006650212706234, 0.02617762660114440407 ) ) ;
#10367 = ORIENTED_EDGE ( 'NONE', *, *, #4311, .F. ) ;
#10368 = VERTEX_POINT ( 'NONE', #3089 ) ;
#10369 = CARTESIAN_POINT ( 'NONE',  ( 0.009374999999999774139, 0.5358532185916217161, 0.06112444011295372487 ) ) ;
#10370 = CARTESIAN_POINT ( 'NONE',  ( -0.2819296736111110424, 4.516055555631421470, -0.1167790944451423119 ) ) ;
#10371 = DIRECTION ( 'NONE',  ( 0.000000000000000000, 0.000000000000000000, -1.000000000000000000 ) ) ;
#10372 = ADVANCED_FACE ( 'NONE', ( #6381 ), #2373, .T. ) ;
#10373 = CARTESIAN_POINT ( 'NONE',  ( 0.3119999999999999996, 3.800777777777776478, -3.820898013339742174E-17 ) ) ;
#10374 = EDGE_CURVE ( 'NONE', #21824, #14703, #7754, .T. ) ;
#10375 = EDGE_CURVE ( 'NONE', #4661, #19679, #892, .T. ) ;
#10376 = COORDINATED_UNIVERSAL_TIME_OFFSET ( 0, 0, .AHEAD. ) ;
#10377 = CARTESIAN_POINT ( 'NONE',  ( 0.3077469291169038779, 0.3525961953783998681, 0.4304954382810343705 ) ) ;
#10378 =( BOUNDED_CURVE ( )  B_SPLINE_CURVE ( 2, ( #4235, #9857, #11573, #22654, #11445, #6061, #11687, #8126, #15577 ),
 .UNSPECIFIED., .F., .F. ) 
 B_SPLINE_CURVE_WITH_KNOTS ( ( 3, 2, 2, 2, 3 ),
 ( 0.7708333333333333703, 0.7812500000000000000, 0.7916666666666666297, 0.8020833333333333703, 0.8125000000000000000 ),
 .UNSPECIFIED. ) 
 CURVE ( )  GEOMETRIC_REPRESENTATION_ITEM ( )  RATIONAL_B_SPLINE_CURVE ( ( 1.000000000000000000, 0.9238795325112867385, 1.000000000000000000, 0.9238795325112867385, 1.000000000000000000, 0.9238795325112867385, 1.000000000000000000, 0.9238795325112867385, 1.000000000000000000 ) ) 
 REPRESENTATION_ITEM ( '' )  );
#10379 = CARTESIAN_POINT ( 'NONE',  ( 0.1954553509668047195, 0.1954553509668046085, 0.01194444444444571485 ) ) ;
#10380 = APPROVAL_PERSON_ORGANIZATION ( #11727, #12871, #11242 ) ;
#10381 = CARTESIAN_POINT ( 'NONE',  ( -0.1993543840281266910, 4.193138888964754507, -0.1993543840281266910 ) ) ;
#10382 = CARTESIAN_POINT ( 'NONE',  ( -0.3111057980080598195, 4.834855633700155586, -0.02361667675171789244 ) ) ;
#10383 = EDGE_CURVE ( 'NONE', #22560, #19497, #11893, .T. ) ;
#10384 = DIRECTION ( 'NONE',  ( 0.6989184867586851757, -0.09025067990440575894, 0.7094841532012832186 ) ) ;
#10385 = CARTESIAN_POINT ( 'NONE',  ( 0.2764156081756483641, -0.1144950937579611028, 0.2306944444444474218 ) ) ;
#10386 = CARTESIAN_POINT ( 'NONE',  ( 0.3613381517857143232, 0.1580357141881718608, -0.1174058825155740587 ) ) ;
#10387 = CARTESIAN_POINT ( 'NONE',  ( 0.2819296736111110979, 0.09097222214635558579, 0.000000000000000000 ) ) ;
#10388 = CARTESIAN_POINT ( 'NONE',  ( 0.4796774003163876143, -0.08638957141560613118, 0.07156364629625895646 ) ) ;
#10389 = CARTESIAN_POINT ( 'NONE',  ( 0.4802530965259536599, 0.2139100642471496172, 0.05348422206366747894 ) ) ;
#10390 = CARTESIAN_POINT ( 'NONE',  ( -0.009375000000000190473, 0.5358532185916217161, 0.06112444011295373181 ) ) ;
#10391 = DIRECTION ( 'NONE',  ( -0.000000000000000000, 1.000000000000000000, -0.000000000000000000 ) ) ;
#10392 = CARTESIAN_POINT ( 'NONE',  ( -0.3155070326520293400, 0.1306872919485614903, 0.3921527777777817914 ) ) ;
#10393 = VERTEX_POINT ( 'NONE', #4552 ) ;
#10394 = DIRECTION ( 'NONE',  ( 0.8660254037844437036, 0.000000000000000000, 0.4999999999999911737 ) ) ;
#10395 = CARTESIAN_POINT ( 'NONE',  ( 0.3125000000000000000, -5.740531871003217465E-17, 0.3661111111111149397 ) ) ;
#10396 = DIRECTION ( 'NONE',  ( -0.4999999999999929501, 0.000000000000000000, -0.8660254037844425934 ) ) ;
#10397 = CARTESIAN_POINT ( 'NONE',  ( -0.2819296736111110979, 0.3444444443685779067, 0.1167790944451422425 ) ) ;
#10398 = CARTESIAN_POINT ( 'NONE',  ( -1.726321361862525858E-17, 4.130638888964754507, -0.2819296736111110979 ) ) ;
#10399 = CARTESIAN_POINT ( 'NONE',  ( 0.2233192592356399997, 0.09374999990245759529, -0.3073725909049500049 ) ) ;
#10400 = ORIENTED_EDGE ( 'NONE', *, *, #12276, .F. ) ;
#10401 = CARTESIAN_POINT ( 'NONE',  ( -0.2819296736111110424, 4.592444444520309865, 0.1167790944451424923 ) ) ;
#10402 = CARTESIAN_POINT ( 'NONE',  ( 0.2431432128212240862, 5.125660135501770576, 0.1885555529197559810 ) ) ;
#10403 = ADVANCED_FACE ( 'NONE', ( #19546 ), #8193, .F. ) ;
#10404 = CARTESIAN_POINT ( 'NONE',  ( 0.2472135954999579166, 0.1660714283763436994, 0.3402603233408160732 ) ) ;
#10405 = EDGE_LOOP ( 'NONE', ( #13360, #9312, #5608, #959 ) ) ;
#10406 = DIRECTION ( 'NONE',  ( 0.000000000000000000, 0.000000000000000000, 1.000000000000000000 ) ) ;
#10407 = CARTESIAN_POINT ( 'NONE',  ( -0.1993543840281266910, 5.123694444520309865, -0.1993543840281266910 ) ) ;
#10408 = CARTESIAN_POINT ( 'NONE',  ( 0.2195630361086305937, -0.1679215936616662852, 0.3880822748423153334 ) ) ;
#10409 = CIRCLE ( 'NONE', #1040, 0.2109499999999995268 ) ;
#10410 = CARTESIAN_POINT ( 'NONE',  ( 0.2658661084243346684, 0.03242967361111057795, 0.09380593400082704036 ) ) ;
#10411 = CARTESIAN_POINT ( 'NONE',  ( 0.2819296736111110979, 4.939666666742532186, -0.1167790944451423396 ) ) ;
#10412 = MECHANICAL_CONTEXT ( 'NONE', #18859, 'mechanical' ) ;
#10413 = ORIENTED_EDGE ( 'NONE', *, *, #18070, .F. ) ;
#10414 = EDGE_CURVE ( 'NONE', #2273, #2833, #23789, .T. ) ;
#10415 = LINE ( 'NONE', #20022, #2390 ) ;
#10416 = CARTESIAN_POINT ( 'NONE',  ( 3.061616997868383018E-17, 0.04579999999999925103, -0.2500000000000000000 ) ) ;
#10417 = ORIENTED_EDGE ( 'NONE', *, *, #16501, .F. ) ;
#10418 = CARTESIAN_POINT ( 'NONE',  ( 0.2819296736111110424, 0.3791666665908000611, 0.1167790944451424923 ) ) ;
#10419 = DIRECTION ( 'NONE',  ( -0.000000000000000000, -1.000000000000000000, -0.000000000000000000 ) ) ;
#10420 = LINE ( 'NONE', #14067, #23598 ) ;
#10421 = CARTESIAN_POINT ( 'NONE',  ( 0.1555449433501408241, 4.076298560705016172, 0.2713454068376597861 ) ) ;
#10422 = CARTESIAN_POINT ( 'NONE',  ( -0.3613381517857144343, 0.1758928570453146822, 0.1174058825155740171 ) ) ;
#10423 = CARTESIAN_POINT ( 'NONE',  ( -0.2736110384480277546, 5.062269768326324026, 0.1517155811448881175 ) ) ;
#10424 = LINE ( 'NONE', #19917, #12379 ) ;
#10425 = AXIS2_PLACEMENT_3D ( 'NONE', #658, #15657, #12377 ) ;
#10426 = ORIENTED_EDGE ( 'NONE', *, *, #16501, .T. ) ;
#10427 = DIRECTION ( 'NONE',  ( 0.000000000000000000, 0.000000000000000000, -1.000000000000000000 ) ) ;
#10428 = CARTESIAN_POINT ( 'NONE',  ( 5.178964085587577574E-17, 3.755638888964754951, 0.2819296736111110979 ) ) ;
#10429 =( BOUNDED_CURVE ( )  B_SPLINE_CURVE ( 2, ( #996, #15994, #10160, #10404, #23172, #19289, #21364, #8423, #21480, #23413, #10514, #17946, #11996 ),
 .UNSPECIFIED., .F., .T. ) 
 B_SPLINE_CURVE_WITH_KNOTS ( ( 3, 2, 2, 2, 2, 2, 3 ),
 ( 0.3928571428571429047, 0.4000000000000000222, 0.4142857142857143127, 0.4285714285714285476, 0.4428571428571428381, 0.4571428571428571286, 0.4642857142857143016 ),
 .UNSPECIFIED. ) 
 CURVE ( )  GEOMETRIC_REPRESENTATION_ITEM ( )  RATIONAL_B_SPLINE_CURVE ( ( 0.9755282581475767101, 0.9755282581475768211, 1.000000000000000000, 0.9510565162951535312, 1.000000000000000000, 0.9510565162951535312, 1.000000000000000000, 0.9510565162951535312, 1.000000000000000000, 0.9510565162951535312, 1.000000000000000000, 0.9755282581475765991, 0.9755282581475767101 ) ) 
 REPRESENTATION_ITEM ( '' )  );
#10430 = CARTESIAN_POINT ( 'NONE',  ( 0.000000000000000000, 0.000000000000000000, -0.1012499999999999928 ) ) ;
#10431 = CARTESIAN_POINT ( 'NONE',  ( 0.2832746799703420026, 5.033777524650573376, -0.1307669425342211644 ) ) ;
#10432 = CARTESIAN_POINT ( 'NONE',  ( 0.2292520601541578884, 5.072999999999999510, 0.2155101067843893659 ) ) ;
#10433 = CARTESIAN_POINT ( 'NONE',  ( -0.03138470014218885940, 4.792977914880279577, 0.3104507266188493153 ) ) ;
#10434 = CARTESIAN_POINT ( 'NONE',  ( -0.1292346314604056745, 4.547305555707287894, -0.3119999999999999996 ) ) ;
#10435 = CARTESIAN_POINT ( 'NONE',  ( 0.1167790944451424506, 4.717444444520309865, 0.2819296736111110424 ) ) ;
#10436 = ORIENTED_EDGE ( 'NONE', *, *, #10048, .F. ) ;
#10437 = CARTESIAN_POINT ( 'NONE',  ( 0.2819296736111110979, 4.047305555631421470, -3.452642723725051716E-17 ) ) ;
#10438 = ORIENTED_EDGE ( 'NONE', *, *, #2081, .F. ) ;
#10439 = CIRCLE ( 'NONE', #1856, 0.01874999999999998890 ) ;
#10440 = APPROVAL_ROLE ( '' ) ;
#10441 = LINE ( 'NONE', #11912, #23533 ) ;
#10442 = DIRECTION ( 'NONE',  ( 0.000000000000000000, -1.000000000000000000, 0.000000000000000000 ) ) ;
#10443 = ORIENTED_EDGE ( 'NONE', *, *, #4151, .F. ) ;
#10444 = CARTESIAN_POINT ( 'NONE',  ( 0.1292346314604056745, 0.1326388887371559577, -0.3119999999999999996 ) ) ;
#10445 = CARTESIAN_POINT ( 'NONE',  ( -0.0002437205570828195761, 4.377173215581007248, -0.3119999107914319114 ) ) ;
#10446 = CARTESIAN_POINT ( 'NONE',  ( 0.1123264932791831761, 3.756093169699424195, -0.3119999999999978346 ) ) ;
#10447 = CARTESIAN_POINT ( 'NONE',  ( 3.061616997868383018E-17, 6.000000000000000888, 0.2500000000000000000 ) ) ;
#10448 = VERTEX_POINT ( 'NONE', #23668 ) ;
#10449 = CARTESIAN_POINT ( 'NONE',  ( -0.1144950937579609918, -0.2764156081756484196, 0.3765277777777819579 ) ) ;
#10450 = CARTESIAN_POINT ( 'NONE',  ( 0.2819296736111110979, 0.03888888881302225015, -0.1167790944451422980 ) ) ;
#10451 = CARTESIAN_POINT ( 'NONE',  ( 0.000000000000000000, 0.2764156081756484196, 0.1300000000000022249 ) ) ;
#10452 = CARTESIAN_POINT ( 'NONE',  ( 0.2819296736111110979, 4.436194444520309865, -3.452642723725051716E-17 ) ) ;
#10453 = CARTESIAN_POINT ( 'NONE',  ( -0.06796888784162306851, 0.2795977689546957357, -0.07675168144635624579 ) ) ;
#10454 = CARTESIAN_POINT ( 'NONE',  ( 0.3950000000000000178, 2.740039370078740433, -2.540999999999999925 ) ) ;
#10455 = CARTESIAN_POINT ( 'NONE',  ( -3.827021247335479543E-17, -0.3125000000000000000, -0.03666666666666597990 ) ) ;
#10456 = CARTESIAN_POINT ( 'NONE',  ( 0.3228671510180489701, 2.690047770615767941, -1.025312217484214639 ) ) ;
#10457 = CARTESIAN_POINT ( 'NONE',  ( 0.2206173157302027954, 4.141055555555554157, -0.2206173157302028232 ) ) ;
#10458 = AXIS2_PLACEMENT_3D ( 'NONE', #12159, #7013, #16278 ) ;
#10459 = CARTESIAN_POINT ( 'NONE',  ( -0.1292346314604056745, 5.102861111262844140, -0.3119999999999999996 ) ) ;
#10460 = CARTESIAN_POINT ( 'NONE',  ( -0.3119999999999999996, 4.661888888888888083, 0.000000000000000000 ) ) ;
#10461 = DIRECTION ( 'NONE',  ( -1.707404996040164512E-16, 0.000000000000000000, 1.000000000000000000 ) ) ;
#10462 = EDGE_LOOP ( 'NONE', ( #2012, #11420, #19086, #1012 ) ) ;
#10463 = CARTESIAN_POINT ( 'NONE',  ( -0.1294417382415922191, 0.3125000000000000000, 0.2237500000000031686 ) ) ;
#10464 = CARTESIAN_POINT ( 'NONE',  ( 0.3155070326520292290, 0.1306872919485615736, 0.04145833333333503318 ) ) ;
#10465 = FACE_OUTER_BOUND ( 'NONE', #18457, .T. ) ;
#10466 = VECTOR ( 'NONE', #12613, 39.37007874015748143 ) ;
#10467 = CARTESIAN_POINT ( 'NONE',  ( 0.000000000000000000, 3.738758431839877614E-19, 0.000000000000000000 ) ) ;
#10468 = CARTESIAN_POINT ( 'NONE',  ( 0.2923287055106771337, 0.1437499999024575981, -0.2123892367102620249 ) ) ;
#10469 = CARTESIAN_POINT ( 'NONE',  ( 1.726321361862525858E-17, 0.6048611110352445364, -0.2819296736111110979 ) ) ;
#10470 = CARTESIAN_POINT ( 'NONE',  ( 0.2764156081756483641, -0.1144950937579611167, -0.04708333333333256793 ) ) ;
#10471 = CARTESIAN_POINT ( 'NONE',  ( 0.1430000000000000993, 2.833000000000000185, -1.917502577388072282 ) ) ;
#10472 = CARTESIAN_POINT ( 'NONE',  ( 0.2819296736111110979, 5.168833333409199149, 0.1167790944451422425 ) ) ;
#10473 = CARTESIAN_POINT ( 'NONE',  ( 0.1954553509668046640, -0.1954553509668047195, 0.4494444444444491427 ) ) ;
#10474 = ORIENTED_EDGE ( 'NONE', *, *, #22139, .T. ) ;
#10475 = CARTESIAN_POINT ( 'NONE',  ( 0.3119999999999999996, 3.856333333333332281, -3.820898013339742174E-17 ) ) ;
#10476 = PLANE ( 'NONE',  #7033 ) ;
#10477 = LINE ( 'NONE', #21798, #5555 ) ;
#10478 = CARTESIAN_POINT ( 'NONE',  ( -0.2206173157302027954, 0.4277777777777774237, -0.2206173157302028232 ) ) ;
#10479 = CARTESIAN_POINT ( 'NONE',  ( 5.731347020009612645E-17, 4.620222222222221120, 0.3119999999999999996 ) ) ;
#10480 = CARTESIAN_POINT ( 'NONE',  ( 0.2819296736111110979, 4.269527777853643791, -3.452642723725051716E-17 ) ) ;
#10481 = CARTESIAN_POINT ( 'NONE',  ( 0.1993543840281266633, 3.901472222298087988, -0.1993543840281266910 ) ) ;
#10482 = CARTESIAN_POINT ( 'NONE',  ( 0.4872114317030045716, 2.291712385858715173, -1.340783969076326132 ) ) ;
#10483 = ORIENTED_EDGE ( 'NONE', *, *, #11697, .F. ) ;
#10484 = VECTOR ( 'NONE', #11571, 39.37007874015748854 ) ;
#10485 = CARTESIAN_POINT ( 'NONE',  ( 0.000000000000000000, 5.384999999999999787, 0.000000000000000000 ) ) ;
#10486 = CARTESIAN_POINT ( 'NONE',  ( -0.1993543840281266910, 4.512583333409199149, -0.1993543840281266910 ) ) ;
#10487 = ADVANCED_FACE ( 'NONE', ( #18438 ), #23548, .T. ) ;
#10488 = CARTESIAN_POINT ( 'NONE',  ( 0.1850421345843279164, -0.2494223792521799987, 0.4217812969067588624 ) ) ;
#10489 = CARTESIAN_POINT ( 'NONE',  ( 0.4687500000000003886, -0.2629256801278681555, 0.05975678175779897128 ) ) ;
#10490 = DATE_AND_TIME ( #16788, #11103 ) ;
#10491 = CARTESIAN_POINT ( 'NONE',  ( -0.4802534626491987146, 0.2139708740945671928, 0.05347073504130966243 ) ) ;
#10492 = CARTESIAN_POINT ( 'NONE',  ( -0.2764156081756484196, 0.1144950937579609918, 0.02930555555555695163 ) ) ;
#10493 = CARTESIAN_POINT ( 'NONE',  ( -0.1167790944451423535, 4.099388888964754507, 0.2819296736111110979 ) ) ;
#10494 = CARTESIAN_POINT ( 'NONE',  ( -0.002180183382288421873, 4.821674524114921923, -0.3119934709836226228 ) ) ;
#10495 = CARTESIAN_POINT ( 'NONE',  ( 0.000000000000000000, 3.700000000000000622, 0.000000000000000000 ) ) ;
#10496 = CARTESIAN_POINT ( 'NONE',  ( -0.1954553509668046918, -0.1954553509668046640, 0.2133333333333361503 ) ) ;
#10497 = CARTESIAN_POINT ( 'NONE',  ( 0.1116596296178199027, -0.002678571526113827667, 0.3436530038418508792 ) ) ;
#10498 = CARTESIAN_POINT ( 'NONE',  ( 0.2819296736111110424, 0.6083333332574668573, -0.1167790944451423119 ) ) ;
#10499 = DIRECTION ( 'NONE',  ( 1.000000000000000000, 0.000000000000000000, 0.000000000000000000 ) ) ;
#10500 = CARTESIAN_POINT ( 'NONE',  ( -0.4795759075923611281, 0.04315783544084986906, 0.07439896364138827434 ) ) ;
#10501 = CARTESIAN_POINT ( 'NONE',  ( -0.06946101865132212061, 0.1664525777826655062, -0.7468903887938297403 ) ) ;
#10502 = CARTESIAN_POINT ( 'NONE',  ( 0.1954553509668046640, -0.1954553509668047195, 0.05361111111111271227 ) ) ;
#10503 = CARTESIAN_POINT ( 'NONE',  ( 0.3155070326520292290, -0.1306872919485616569, 0.4199305555555598590 ) ) ;
#10504 = VERTEX_POINT ( 'NONE', #16256 ) ;
#10505 = ORIENTED_EDGE ( 'NONE', *, *, #14237, .F. ) ;
#10506 = CARTESIAN_POINT ( 'NONE',  ( -4.638126268221291196E-16, 0.06071428571428570675, -0.4000000000000000222 ) ) ;
#10507 = CARTESIAN_POINT ( 'NONE',  ( 1.726321361862525858E-17, 0.6048611110352445364, -0.2819296736111110979 ) ) ;
#10508 = CARTESIAN_POINT ( 'NONE',  ( 0.1993543840281266355, 0.4173611110352444808, 0.1993543840281267465 ) ) ;
#10509 = EDGE_CURVE ( 'NONE', #6154, #19422, #24035, .T. ) ;
#10510 = CARTESIAN_POINT ( 'NONE',  ( -0.2819296736111110424, 3.981333333409199593, 0.1167790944451424923 ) ) ;
#10511 = CARTESIAN_POINT ( 'NONE',  ( 0.1116596296178199860, 0.02589285704531474330, -0.3436530038418508792 ) ) ;
#10512 = CARTESIAN_POINT ( 'NONE',  ( -0.2819296736111110424, 4.585500000075865223, -0.1167790944451423119 ) ) ;
#10513 = CARTESIAN_POINT ( 'NONE',  ( 0.07964491704986943754, 5.141321981404664676, -0.2945216132760368200 ) ) ;
#10514 = CARTESIAN_POINT ( 'NONE',  ( 0.1236067977499789861, 0.1910714283763437493, -0.3804226065180614236 ) ) ;
#10515 = ORIENTED_EDGE ( 'NONE', *, *, #3643, .T. ) ;
#10516 = FACE_OUTER_BOUND ( 'NONE', #3534, .T. ) ;
#10517 = CARTESIAN_POINT ( 'NONE',  ( 0.1123265699853363830, 3.707482056679137550, -0.3120000000000000551 ) ) ;
#10518 = ADVANCED_FACE ( 'NONE', ( #14429 ), #8932, .F. ) ;
#10519 = DIRECTION ( 'NONE',  ( 0.000000000000000000, 0.000000000000000000, -1.000000000000000000 ) ) ;
#10520 = AXIS2_PLACEMENT_3D ( 'NONE', #19069, #2253, #2377 ) ;
#10521 = ORIENTED_EDGE ( 'NONE', *, *, #10998, .T. ) ;
#10522 = CARTESIAN_POINT ( 'NONE',  ( -0.1167790944451423119, 4.898000000075865223, -0.2819296736111110979 ) ) ;
#10523 = DATE_AND_TIME ( #6493, #4511 ) ;
#10524 = ORIENTED_EDGE ( 'NONE', *, *, #6277, .F. ) ;
#10525 = CARTESIAN_POINT ( 'NONE',  ( -0.1292346314604056190, 0.3062499998482671182, -0.3119999999999999996 ) ) ;
#10526 = CARTESIAN_POINT ( 'NONE',  ( 1.910449006669871087E-17, 0.2541666666666663188, -0.3119999999999999996 ) ) ;
#10527 = VERTEX_POINT ( 'NONE', #7109 ) ;
#10528 = CARTESIAN_POINT ( 'NONE',  ( 0.1167790944451423257, 0.2819444443685777957, -0.2819296736111110424 ) ) ;
#10529 = ORIENTED_EDGE ( 'NONE', *, *, #199, .F. ) ;
#10530 = LINE ( 'NONE', #2962, #6272 ) ;
#10531 = CARTESIAN_POINT ( 'NONE',  ( -0.3120000000000000551, 0.3270833333333330040, 0.1292346314604056190 ) ) ;
#10532 = CARTESIAN_POINT ( 'NONE',  ( 0.05000000000000028727, 2.740000000000000213, 0.000000000000000000 ) ) ;
#10533 = CARTESIAN_POINT ( 'NONE',  ( -7.726019084026502927E-17, 0.02499999999999997363, 0.4205848896953069405 ) ) ;
#10534 = CARTESIAN_POINT ( 'NONE',  ( -0.2867585069081046156, 5.054137861884946403, -0.1229525427538243343 ) ) ;
#10535 = DIRECTION ( 'NONE',  ( -0.000000000000000000, 0.9767851838303063250, 0.2142211582677935044 ) ) ;
#10536 = EDGE_CURVE ( 'NONE', #10074, #10173, #11722, .T. ) ;
#10537 = CARTESIAN_POINT ( 'NONE',  ( 6.402768735150616610E-17, -0.5196152422706635798, 0.3779506566538943235 ) ) ;
#10538 = AXIS2_PLACEMENT_3D ( 'NONE', #21663, #18009, #23595 ) ;
#10539 = CARTESIAN_POINT ( 'NONE',  ( -0.1993543840281266910, 4.804250000075865223, -0.1993543840281266910 ) ) ;
#10540 = CARTESIAN_POINT ( 'NONE',  ( -4.638126268221291196E-16, 0.1232142855192009251, -0.4000000000000000222 ) ) ;
#10541 = CARTESIAN_POINT ( 'NONE',  ( -1.726321361862525858E-17, 3.727861111186976384, -0.2819296736111110979 ) ) ;
#10542 = FACE_OUTER_BOUND ( 'NONE', #348, .T. ) ;
#10543 = CARTESIAN_POINT ( 'NONE',  ( 0.2874842063055126351, 5.033475709842507584, -0.1212575126306435908 ) ) ;
#10544 = CARTESIAN_POINT ( 'NONE',  ( -0.5116234456863258950, 1.999640111863030256, -2.845780280100675963 ) ) ;
#10545 = DIRECTION ( 'NONE',  ( -0.7745966692414841814, -0.4472135954999572061, -0.4472135954999572061 ) ) ;
#10546 = CARTESIAN_POINT ( 'NONE',  ( 0.1292346314604056190, 4.207027777929510215, -0.3119999999999999996 ) ) ;
#10547 = EDGE_CURVE ( 'NONE', #15596, #14458, #11454, .T. ) ;
#10548 = CARTESIAN_POINT ( 'NONE',  ( -0.1993543840281266910, 4.693138888964754507, -0.1993543840281266910 ) ) ;
#10549 = ORIENTED_EDGE ( 'NONE', *, *, #6164, .T. ) ;
#10550 = CARTESIAN_POINT ( 'NONE',  ( 0.1993543840281266633, 3.943138888964754507, -0.1993543840281266910 ) ) ;
#10551 = EDGE_LOOP ( 'NONE', ( #19933, #6089, #2371, #11286 ) ) ;
#10552 = ORIENTED_EDGE ( 'NONE', *, *, #2438, .F. ) ;
#10553 = VECTOR ( 'NONE', #9923, 39.37007874015748143 ) ;
#10554 = AXIS2_PLACEMENT_3D ( 'NONE', #22033, #20213, #21551 ) ;
#10555 = ORIENTED_EDGE ( 'NONE', *, *, #14503, .F. ) ;
#10556 = APPROVAL_DATE_TIME ( #21513, #16697 ) ;
#10557 = CARTESIAN_POINT ( 'NONE',  ( 0.1292346314604056190, 4.255638888888888083, -0.3119999999999999996 ) ) ;
#10558 = DIRECTION ( 'NONE',  ( 0.8660254037844435926, 0.000000000000000000, -0.4999999999999914513 ) ) ;
#10559 = ORIENTED_EDGE ( 'NONE', *, *, #13293, .T. ) ;
#10560 = CARTESIAN_POINT ( 'NONE',  ( -0.2206173157302028787, 0.3791666665149337478, 0.2206173157302027954 ) ) ;
#10561 = CARTESIAN_POINT ( 'NONE',  ( -6.389700406101856968E-07, 4.404919069638722817, 0.3119999999986028949 ) ) ;
#10562 = CARTESIAN_POINT ( 'NONE',  ( -0.4687500000000003886, 0.04410323065863043512, 0.4181500734908987771 ) ) ;
#10563 = CARTESIAN_POINT ( 'NONE',  ( -0.3999999999999999667, 0.3607142857142855430, -0.1299678784931626030 ) ) ;
#10564 =( BOUNDED_SURFACE ( )  B_SPLINE_SURFACE ( 1, 2, ( 
 ( #21517, #15443, #4578, #23330, #6643, #8469, #19690, #798, #17625, #6283, #22869, #11916, #13738, #15676, #21161, #23094, #19208, #4807, #2516, #4692, #8104, #17386, #19568, #2993, #2749, #554, #915, #10200, #14090, #15796, #19335, #23215, #2858, #12274, #9958, #10444, #7991, #21042, #10319, #681, #17745, #4452, #2632, #10081, #17501, #21881, #8832, #5049, #20180, #7258, #12885, #14210, #9076, #18347, #16280, #22000, #14331, #16407, #3226, #23455, #1405, #5172, #18230, #7137, #14704, #22120, #16160, #21764, #14577, #12519, #23576, #23692, #12639, #23815, #19938, #10918, #10674, #5300, #12762, #6889, #20300, #21643, #5418, #3585, #1641, #17870, #1527, #3468, #17992, #18108, #16524, #23942, #7015, #14459, #1161, #20058, #3348, #10801, #8602, #16041, #6764, #8959, #4932, #12398, #19815, #3111, #10560, #1284, #8709, #1759, #167, #9683, #17122, #18951, #6010, #11275, #3951, #16761, #9203, #22356, #44, #18707, #7490, #2005, #5539, #15291, #22240, #15173, #18588, #3711, #22608, #13478, #5778, #11037, #11394, #22482, #410, #9442, #5660, #18826, #7608, #2249, #20416, #7844, #18467, #22720, #286, #16644, #14823, #13240, #16877, #9561, #20653, #20893, #16994, #24063, #7373, #3835, #14937, #20539, #13003, #11160, #5892, #1880, #15060, #9321, #13124, #2120, #7727, #13352, #20774, #4063, #11518, #8319, #11760, #21010, #15770, #6614, #23068, #4187, #21259 ),
 ( #19542, #13597, #1011, #11640, #2834, #17598, #9809, #7961, #15649, #10052, #2721, #13825, #10293, #10174, #23304, #8441, #21134, #8077, #13714, #17242, #524, #23189, #17716, #17476, #15413, #17358, #4547, #12010, #15530, #6377, #22951, #14063, #8200, #19304, #6254, #6499, #15886, #19065, #22841, #2372, #4666, #2608, #13946, #650, #888, #4424, #6129, #11889, #19423, #21376, #12134, #4303, #19182, #2491, #768, #9927, #8681, #3086, #5021, #16253, #20025, #16130, #14545, #23545, #1492, #3314, #19785, #23905, #1134, #10887, #16494, #21967, #21492, #5140, #18197, #21612, #6860, #10771, #8928, #14302, #3195, #16374, #8803, #10528, #12486, #5261, #23784, #7106, #12605, #12732, #23663, #3435, #18074, #21736, #19906, #18316, #12248, #10642, #20148, #1613, #9047, #7223, #1374, #14426, #17959, #19662, #6982, #1252, #21851, #4781, #2960, #10418, #17841, #8567, #16008, #23427, #6737, #14179, #4906, #12368, #22208, #135, #15026, #4035, #9652, #16610, #20506, #7578, #16963, #5626, #15144, #9530, #11489, #8, #13210, #24030, #3801, #12850, #7456, #20268, #18793, #14905, #22451, #378, #22326, #9410, #258, #14792, #18553, #1728, #22574, #3678, #17090, #1842, #13092, #11124, #2221, #2088, #5750, #20621, #5507, #12970, #9166, #16728, #7340, #22089, #11245, #9285, #18672, #1972, #16848, #3921, #20386, #11366, #7698, #5862, #13321, #20743, #18921, #14670, #5384 ) ),
 .UNSPECIFIED., .F., .F., .T. ) 
 B_SPLINE_SURFACE_WITH_KNOTS ( ( 2, 2 ),
 ( 3, 2, 2, 2, 2, 2, 2, 2, 2, 2, 2, 2, 2, 2, 2, 2, 2, 2, 2, 2, 2, 2, 2, 2, 2, 2, 2, 2, 2, 2, 2, 2, 2, 2, 2, 2, 2, 2, 2, 2, 2, 2, 2, 2, 2, 2, 2, 2, 2, 2, 2, 2, 2, 2, 2, 2, 2, 2, 2, 2, 2, 2, 2, 2, 2, 2, 2, 2, 2, 2, 2, 2, 2, 2, 2, 2, 2, 2, 2, 2, 2, 2, 2, 2, 2, 2, 2, 2, 2, 2, 3 ),
 ( 0.000000000000000000, 1.000000000000000000 ),
 ( 0.000000000000000000, 0.01041666666666666609, 0.02083333333333333218, 0.03125000000000000000, 0.04166666666666666435, 0.05208333333333333565, 0.06250000000000000000, 0.07291666666666667129, 0.08333333333333332871, 0.09375000000000000000, 0.1041666666666666713, 0.1145833333333333287, 0.1250000000000000000, 0.1354166666666666574, 0.1458333333333333426, 0.1562500000000000000, 0.1666666666666666574, 0.1770833333333333426, 0.1875000000000000000, 0.1979166666666666574, 0.2083333333333333426, 0.2187500000000000000, 0.2291666666666666574, 0.2395833333333333426, 0.2500000000000000000, 0.2604166666666666852, 0.2708333333333333148, 0.2812500000000000000, 0.2916666666666666852, 0.3020833333333333148, 0.3125000000000000000, 0.3229166666666666852, 0.3333333333333333148, 0.3437500000000000000, 0.3541666666666666852, 0.3645833333333333148, 0.3750000000000000000, 0.3854166666666666852, 0.3958333333333333148, 0.4062500000000000000, 0.4166666666666666852, 0.4270833333333333148, 0.4375000000000000000, 0.4479166666666666852, 0.4583333333333333148, 0.4687500000000000000, 0.4791666666666666852, 0.4895833333333333148, 0.5000000000000000000, 0.5104166666666666297, 0.5208333333333333703, 0.5312500000000000000, 0.5416666666666666297, 0.5520833333333333703, 0.5625000000000000000, 0.5729166666666666297, 0.5833333333333333703, 0.5937500000000000000, 0.6041666666666666297, 0.6145833333333333703, 0.6250000000000000000, 0.6354166666666666297, 0.6458333333333333703, 0.6562500000000000000, 0.6666666666666666297, 0.6770833333333333703, 0.6875000000000000000, 0.6979166666666666297, 0.7083333333333333703, 0.7187500000000000000, 0.7291666666666666297, 0.7395833333333333703, 0.7500000000000000000, 0.7604166666666666297, 0.7708333333333333703, 0.7812500000000000000, 0.7916666666666666297, 0.8020833333333333703, 0.8125000000000000000, 0.8229166666666666297, 0.8333333333333333703, 0.8437500000000000000, 0.8541666666666666297, 0.8645833333333333703, 0.8750000000000000000, 0.8854166666666666297, 0.8958333333333333703, 0.9062500000000000000, 0.9166666666666666297, 0.9270833333333333703, 0.9375000000000000000 ),
 .UNSPECIFIED. ) 
 GEOMETRIC_REPRESENTATION_ITEM ( )  RATIONAL_B_SPLINE_SURFACE ( (
 ( 1.000000000000000000, 0.9238795325112867385, 1.000000000000000000, 0.9238795325112867385, 1.000000000000000000, 0.9238795325112867385, 1.000000000000000000, 0.9238795325112867385, 1.000000000000000000, 0.9238795325112867385, 1.000000000000000000, 0.9238795325112867385, 1.000000000000000000, 0.9238795325112867385, 1.000000000000000000, 0.9238795325112867385, 1.000000000000000000, 0.9238795325112867385, 1.000000000000000000, 0.9238795325112867385, 1.000000000000000000, 0.9238795325112867385, 1.000000000000000000, 0.9238795325112867385, 1.000000000000000000, 0.9238795325112867385, 1.000000000000000000, 0.9238795325112867385, 1.000000000000000000, 0.9238795325112867385, 1.000000000000000000, 0.9238795325112867385, 1.000000000000000000, 0.9238795325112867385, 1.000000000000000000, 0.9238795325112867385, 1.000000000000000000, 0.9238795325112867385, 1.000000000000000000, 0.9238795325112867385, 1.000000000000000000, 0.9238795325112867385, 1.000000000000000000, 0.9238795325112867385, 1.000000000000000000, 0.9238795325112867385, 1.000000000000000000, 0.9238795325112867385, 1.000000000000000000, 0.9238795325112867385, 1.000000000000000000, 0.9238795325112867385, 1.000000000000000000, 0.9238795325112867385, 1.000000000000000000, 0.9238795325112867385, 1.000000000000000000, 0.9238795325112867385, 1.000000000000000000, 0.9238795325112867385, 1.000000000000000000, 0.9238795325112867385, 1.000000000000000000, 0.9238795325112867385, 1.000000000000000000, 0.9238795325112867385, 1.000000000000000000, 0.9238795325112867385, 1.000000000000000000, 0.9238795325112867385, 1.000000000000000000, 0.9238795325112867385, 1.000000000000000000, 0.9238795325112867385, 1.000000000000000000, 0.9238795325112867385, 1.000000000000000000, 0.9238795325112867385, 1.000000000000000000, 0.9238795325112867385, 1.000000000000000000, 0.9238795325112867385, 1.000000000000000000, 0.9238795325112867385, 1.000000000000000000, 0.9238795325112867385, 1.000000000000000000, 0.9238795325112867385, 1.000000000000000000, 0.9238795325112867385, 1.000000000000000000, 0.9238795325112867385, 1.000000000000000000, 0.9238795325112867385, 1.000000000000000000, 0.9238795325112867385, 1.000000000000000000, 0.9238795325112867385, 1.000000000000000000, 0.9238795325112867385, 1.000000000000000000, 0.9238795325112867385, 1.000000000000000000, 0.9238795325112867385, 1.000000000000000000, 0.9238795325112867385, 1.000000000000000000, 0.9238795325112867385, 1.000000000000000000, 0.9238795325112867385, 1.000000000000000000, 0.9238795325112867385, 1.000000000000000000, 0.9238795325112867385, 1.000000000000000000, 0.9238795325112867385, 1.000000000000000000, 0.9238795325112867385, 1.000000000000000000, 0.9238795325112867385, 1.000000000000000000, 0.9238795325112867385, 1.000000000000000000, 0.9238795325112867385, 1.000000000000000000, 0.9238795325112867385, 1.000000000000000000, 0.9238795325112867385, 1.000000000000000000, 0.9238795325112867385, 1.000000000000000000, 0.9238795325112867385, 1.000000000000000000, 0.9238795325112867385, 1.000000000000000000, 0.9238795325112867385, 1.000000000000000000, 0.9238795325112867385, 1.000000000000000000, 0.9238795325112867385, 1.000000000000000000, 0.9238795325112867385, 1.000000000000000000, 0.9238795325112867385, 1.000000000000000000, 0.9238795325112867385, 1.000000000000000000, 0.9238795325112867385, 1.000000000000000000, 0.9238795325112867385, 1.000000000000000000, 0.9238795325112867385, 1.000000000000000000, 0.9238795325112867385, 1.000000000000000000, 0.9238795325112867385, 1.000000000000000000, 0.9238795325112867385, 1.000000000000000000, 0.9238795325112867385, 1.000000000000000000, 0.9238795325112867385, 1.000000000000000000, 0.9238795325112867385, 1.000000000000000000, 0.9238795325112867385, 1.000000000000000000, 0.9238795325112867385, 1.000000000000000000, 0.9238795325112867385, 1.000000000000000000, 0.9238795325112867385, 1.000000000000000000, 0.9238795325112867385, 1.000000000000000000, 0.9238795325112867385, 1.000000000000000000, 0.9238795325112867385, 1.000000000000000000, 0.9238795325112867385, 1.000000000000000000),
 ( 1.000000000000000000, 0.9238795325112867385, 1.000000000000000000, 0.9238795325112867385, 1.000000000000000000, 0.9238795325112867385, 1.000000000000000000, 0.9238795325112867385, 1.000000000000000000, 0.9238795325112867385, 1.000000000000000000, 0.9238795325112867385, 1.000000000000000000, 0.9238795325112867385, 1.000000000000000000, 0.9238795325112867385, 1.000000000000000000, 0.9238795325112867385, 1.000000000000000000, 0.9238795325112867385, 1.000000000000000000, 0.9238795325112867385, 1.000000000000000000, 0.9238795325112867385, 1.000000000000000000, 0.9238795325112867385, 1.000000000000000000, 0.9238795325112867385, 1.000000000000000000, 0.9238795325112867385, 1.000000000000000000, 0.9238795325112867385, 1.000000000000000000, 0.9238795325112867385, 1.000000000000000000, 0.9238795325112867385, 1.000000000000000000, 0.9238795325112867385, 1.000000000000000000, 0.9238795325112867385, 1.000000000000000000, 0.9238795325112867385, 1.000000000000000000, 0.9238795325112867385, 1.000000000000000000, 0.9238795325112867385, 1.000000000000000000, 0.9238795325112867385, 1.000000000000000000, 0.9238795325112867385, 1.000000000000000000, 0.9238795325112867385, 1.000000000000000000, 0.9238795325112867385, 1.000000000000000000, 0.9238795325112867385, 1.000000000000000000, 0.9238795325112867385, 1.000000000000000000, 0.9238795325112867385, 1.000000000000000000, 0.9238795325112867385, 1.000000000000000000, 0.9238795325112867385, 1.000000000000000000, 0.9238795325112867385, 1.000000000000000000, 0.9238795325112867385, 1.000000000000000000, 0.9238795325112867385, 1.000000000000000000, 0.9238795325112867385, 1.000000000000000000, 0.9238795325112867385, 1.000000000000000000, 0.9238795325112867385, 1.000000000000000000, 0.9238795325112867385, 1.000000000000000000, 0.9238795325112867385, 1.000000000000000000, 0.9238795325112867385, 1.000000000000000000, 0.9238795325112867385, 1.000000000000000000, 0.9238795325112867385, 1.000000000000000000, 0.9238795325112867385, 1.000000000000000000, 0.9238795325112867385, 1.000000000000000000, 0.9238795325112867385, 1.000000000000000000, 0.9238795325112867385, 1.000000000000000000, 0.9238795325112867385, 1.000000000000000000, 0.9238795325112867385, 1.000000000000000000, 0.9238795325112867385, 1.000000000000000000, 0.9238795325112867385, 1.000000000000000000, 0.9238795325112867385, 1.000000000000000000, 0.9238795325112867385, 1.000000000000000000, 0.9238795325112867385, 1.000000000000000000, 0.9238795325112867385, 1.000000000000000000, 0.9238795325112867385, 1.000000000000000000, 0.9238795325112867385, 1.000000000000000000, 0.9238795325112867385, 1.000000000000000000, 0.9238795325112867385, 1.000000000000000000, 0.9238795325112867385, 1.000000000000000000, 0.9238795325112867385, 1.000000000000000000, 0.9238795325112867385, 1.000000000000000000, 0.9238795325112867385, 1.000000000000000000, 0.9238795325112867385, 1.000000000000000000, 0.9238795325112867385, 1.000000000000000000, 0.9238795325112867385, 1.000000000000000000, 0.9238795325112867385, 1.000000000000000000, 0.9238795325112867385, 1.000000000000000000, 0.9238795325112867385, 1.000000000000000000, 0.9238795325112867385, 1.000000000000000000, 0.9238795325112867385, 1.000000000000000000, 0.9238795325112867385, 1.000000000000000000, 0.9238795325112867385, 1.000000000000000000, 0.9238795325112867385, 1.000000000000000000, 0.9238795325112867385, 1.000000000000000000, 0.9238795325112867385, 1.000000000000000000, 0.9238795325112867385, 1.000000000000000000, 0.9238795325112867385, 1.000000000000000000, 0.9238795325112867385, 1.000000000000000000, 0.9238795325112867385, 1.000000000000000000, 0.9238795325112867385, 1.000000000000000000, 0.9238795325112867385, 1.000000000000000000, 0.9238795325112867385, 1.000000000000000000, 0.9238795325112867385, 1.000000000000000000, 0.9238795325112867385, 1.000000000000000000, 0.9238795325112867385, 1.000000000000000000, 0.9238795325112867385, 1.000000000000000000, 0.9238795325112867385, 1.000000000000000000, 0.9238795325112867385, 1.000000000000000000, 0.9238795325112867385, 1.000000000000000000) ) ) 
 REPRESENTATION_ITEM ( '' )  SURFACE ( )  );
#10565 = EDGE_LOOP ( 'NONE', ( #17314, #10709, #15233, #9196, #4622 ) ) ;
#10566 =( BOUNDED_CURVE ( )  B_SPLINE_CURVE ( 2, ( #17126, #7848, #11398, #415, #11644, #291, #6014, #9813, #17246 ),
 .UNSPECIFIED., .F., .T. ) 
 B_SPLINE_CURVE_WITH_KNOTS ( ( 3, 2, 2, 2, 3 ),
 ( 0.8541666666666666297, 0.8645833333333333703, 0.8750000000000000000, 0.8854166666666666297, 0.8958333333333333703 ),
 .UNSPECIFIED. ) 
 CURVE ( )  GEOMETRIC_REPRESENTATION_ITEM ( )  RATIONAL_B_SPLINE_CURVE ( ( 1.000000000000000000, 0.9238795325112867385, 1.000000000000000000, 0.9238795325112867385, 1.000000000000000000, 0.9238795325112867385, 1.000000000000000000, 0.9238795325112867385, 1.000000000000000000 ) ) 
 REPRESENTATION_ITEM ( '' )  );
#10567 = ORIENTED_EDGE ( 'NONE', *, *, #19683, .T. ) ;
#10568 = CARTESIAN_POINT ( 'NONE',  ( 0.000000000000000000, 5.579732050807569621, 0.000000000000000000 ) ) ;
#10569 = DIRECTION ( 'NONE',  ( 0.000000000000000000, 0.000000000000000000, 1.000000000000000000 ) ) ;
#10570 = CARTESIAN_POINT ( 'NONE',  ( 0.2764156081756483641, 0.1144950937579610056, 0.1195833333333354703 ) ) ;
#10571 = CARTESIAN_POINT ( 'NONE',  ( 0.2819296736111110979, 4.491750000075865223, -3.452642723725051716E-17 ) ) ;
#10572 = CARTESIAN_POINT ( 'NONE',  ( 0.2245903949464508609, 0.1902879574984975564, -0.08291343549538147950 ) ) ;
#10573 = CARTESIAN_POINT ( 'NONE',  ( -0.2732709761971058859, 0.6284990011602862303, -1.089116489376853014 ) ) ;
#10574 = CARTESIAN_POINT ( 'NONE',  ( -0.2209708691207961373, -0.2209708691207961095, -0.04361111111111047600 ) ) ;
#10575 = CARTESIAN_POINT ( 'NONE',  ( -0.3100951778434036243, 4.225344069393538682, 0.03479879867075674066 ) ) ;
#10576 = CARTESIAN_POINT ( 'NONE',  ( 0.1292346314604058410, 4.012583333333332725, 0.3119999999999998885 ) ) ;
#10577 = AXIS2_PLACEMENT_3D ( 'NONE', #7914, #15365, #6088 ) ;
#10578 = EDGE_CURVE ( 'NONE', #9622, #15906, #7821, .T. ) ;
#10579 = CARTESIAN_POINT ( 'NONE',  ( -0.1292346314604057023, 5.068138889040620931, 0.3119999999999998885 ) ) ;
#10580 = EDGE_CURVE ( 'NONE', #17016, #11636, #21309, .T. ) ;
#10581 = CARTESIAN_POINT ( 'NONE',  ( -0.3125000000000000000, 1.913510623667739771E-17, 0.2272222222222250176 ) ) ;
#10582 = VERTEX_POINT ( 'NONE', #11370 ) ;
#10583 = CARTESIAN_POINT ( 'NONE',  ( -1.858121103377620624E-07, 4.877166671810766019, -0.3119999999999446549 ) ) ;
#10584 = CARTESIAN_POINT ( 'NONE',  ( 0.2230971623002954429, 0.2230971623002953319, 0.04493055555555729857 ) ) ;
#10585 = CARTESIAN_POINT ( 'NONE',  ( 0.1116596296178199027, 0.4258928570453147100, 0.3436530038418508792 ) ) ;
#10586 = CARTESIAN_POINT ( 'NONE',  ( 0.03174294256098301320, 2.685901063997346405, -0.8524985337548631747 ) ) ;
#10587 = CARTESIAN_POINT ( 'NONE',  ( 0.2233192592356399997, 0.2187499999024575814, -0.3073725909049500049 ) ) ;
#10588 = CARTESIAN_POINT ( 'NONE',  ( -1.949169748562458500E-16, 0.5196152422706634688, 0.3779506566538943790 ) ) ;
#10589 = CARTESIAN_POINT ( 'NONE',  ( -0.2764156081756484196, 0.1144950937579609918, -0.01930555555555454883 ) ) ;
#10590 = CARTESIAN_POINT ( 'NONE',  ( -0.1167790944451423535, 5.210500000075866112, 0.2819296736111110424 ) ) ;
#10591 = CARTESIAN_POINT ( 'NONE',  ( 0.2764156081756483641, 0.1144950937579610056, 0.4598611111111158833 ) ) ;
#10592 = ORIENTED_EDGE ( 'NONE', *, *, #10668, .F. ) ;
#10593 = CC_DESIGN_PERSON_AND_ORGANIZATION_ASSIGNMENT ( #1754, #20295, ( #13854 ) ) ;
#10594 = CARTESIAN_POINT ( 'NONE',  ( -0.04876738698855743320, 4.292444203642808098, 0.3083149109922141973 ) ) ;
#10595 = DIRECTION ( 'NONE',  ( 0.000000000000000000, 0.000000000000000000, -1.000000000000000000 ) ) ;
#10596 = CARTESIAN_POINT ( 'NONE',  ( -0.3119999999999999996, 0.4868055555555551583, -0.1292346314604056745 ) ) ;
#10597 = CARTESIAN_POINT ( 'NONE',  ( -0.2206173157302027676, 4.779944444444443441, 0.2206173157302028787 ) ) ;
#10598 = CARTESIAN_POINT ( 'NONE',  ( -0.1993543840281266910, 4.234805555631421470, -0.1993543840281266910 ) ) ;
#10599 = CARTESIAN_POINT ( 'NONE',  ( -5.731347020009612645E-17, 0.4416666665149336923, 0.3119999999999999996 ) ) ;
#10600 = CARTESIAN_POINT ( 'NONE',  ( 1.020000000000000018, 2.740039370078740433, -2.591000000000000192 ) ) ;
#10601 = LINE ( 'NONE', #12685, #14064 ) ;
#10602 = EDGE_LOOP ( 'NONE', ( #9936, #14124, #21281, #11111 ) ) ;
#10603 = CARTESIAN_POINT ( 'NONE',  ( 0.009375000000000067307, -0.5358532185916218271, 0.06112444011295370405 ) ) ;
#10604 = CARTESIAN_POINT ( 'NONE',  ( 0.2819296736111110979, 4.599388888964753619, 0.1167790944451422425 ) ) ;
#10605 = FACE_OUTER_BOUND ( 'NONE', #21009, .T. ) ;
#10606 = PERSON_AND_ORGANIZATION_ROLE ( 'design_owner' ) ;
#10607 = DIRECTION ( 'NONE',  ( -0.8459207832372978020, 0.4883925919151543282, 0.2142211582677917281 ) ) ;
#10608 = EDGE_CURVE ( 'NONE', #15341, #8827, #14773, .T. ) ;
#10609 = CARTESIAN_POINT ( 'NONE',  ( 0.1954553509668046640, -0.1954553509668047195, 0.1091666666666687158 ) ) ;
#10610 = CARTESIAN_POINT ( 'NONE',  ( 0.1167790944451424506, 4.161888888964755395, 0.2819296736111110424 ) ) ;
#10611 = CARTESIAN_POINT ( 'NONE',  ( -0.3125000000000002776, 0.1294417382415919970, -0.05402777777777723056 ) ) ;
#10612 = DIRECTION ( 'NONE',  ( 0.000000000000000000, 0.000000000000000000, -1.000000000000000000 ) ) ;
#10613 = CARTESIAN_POINT ( 'NONE',  ( -0.1144950937579609779, 0.2764156081756484196, 0.1959722222222249899 ) ) ;
#10614 = CARTESIAN_POINT ( 'NONE',  ( -0.2233192592356399997, 0.1294642856167433076, 0.3073725909049499494 ) ) ;
#10615 = CARTESIAN_POINT ( 'NONE',  ( -0.2819296736111110424, 0.5736111110352444253, -0.1167790944451423396 ) ) ;
#10616 = CARTESIAN_POINT ( 'NONE',  ( 0.1294417382415924134, 0.3124999999999999445, -0.06097222222222135196 ) ) ;
#10617 = DIRECTION ( 'NONE',  ( -0.000000000000000000, -1.000000000000000000, -0.000000000000000000 ) ) ;
#10618 = CC_DESIGN_DATE_AND_TIME_ASSIGNMENT ( #19810, #10314, ( #5667 ) ) ;
#10619 = CARTESIAN_POINT ( 'NONE',  ( -0.1741657073137734824, 0.2450887835488839428, -0.7295075619333545314 ) ) ;
#10620 = CARTESIAN_POINT ( 'NONE',  ( 0.000000000000000000, 0.2764156081756484196, 0.1300000000000022249 ) ) ;
#10621 = CARTESIAN_POINT ( 'NONE',  ( 0.000000000000000000, 0.3155070326520292845, 0.4372916666666711305 ) ) ;
#10622 = ORIENTED_EDGE ( 'NONE', *, *, #23606, .T. ) ;
#10623 = CARTESIAN_POINT ( 'NONE',  ( -0.3236067977499790249, 0.08571428571428568732, 0.2351141009169892271 ) ) ;
#10624 = EDGE_CURVE ( 'NONE', #10349, #21451, #13067, .T. ) ;
#10625 = CARTESIAN_POINT ( 'NONE',  ( 0.4687500000000002776, 0.2178650770398900538, 0.3900584262746596420 ) ) ;
#10626 = CARTESIAN_POINT ( 'NONE',  ( -0.2819296736111110424, 0.3930555554796889561, -0.1167790944451423396 ) ) ;
#10627 = CARTESIAN_POINT ( 'NONE',  ( 0.2819296736111110979, 3.894527777853643347, -3.452642723725051716E-17 ) ) ;
#10628 = CARTESIAN_POINT ( 'NONE',  ( 2.326421213736078119E-17, -0.04196428581182809481, -0.3799334167787516425 ) ) ;
#10629 = CARTESIAN_POINT ( 'NONE',  ( -0.1167790944451423257, 4.523000000075867000, -0.2819296736111110424 ) ) ;
#10630 = CARTESIAN_POINT ( 'NONE',  ( 0.1355903456263229667, 5.139740703596304527, -0.2731414004538880724 ) ) ;
#10631 = CARTESIAN_POINT ( 'NONE',  ( -0.2206173157302027676, 4.613277777777776478, 0.2206173157302028787 ) ) ;
#10632 = ORIENTED_EDGE ( 'NONE', *, *, #18094, .F. ) ;
#10633 = DIRECTION ( 'NONE',  ( -0.000000000000000000, -1.000000000000000000, -0.000000000000000000 ) ) ;
#10634 = CARTESIAN_POINT ( 'NONE',  ( 0.1993543840281267465, 5.151472222298087544, 0.1993543840281266633 ) ) ;
#10635 = CARTESIAN_POINT ( 'NONE',  ( 0.1971119857566866196, 4.204467586177645266, -0.2422589368263572407 ) ) ;
#10636 = CARTESIAN_POINT ( 'NONE',  ( 0.2819296736111111534, 4.821611111186976828, 0.1167790944451422563 ) ) ;
#10637 = APPROVAL_ROLE ( '' ) ;
#10638 = VECTOR ( 'NONE', #13227, 39.37007874015748854 ) ;
#10639 = CARTESIAN_POINT ( 'NONE',  ( -5.731347020009612645E-17, 0.3305555554038226429, 0.3119999999999999996 ) ) ;
#10640 = CARTESIAN_POINT ( 'NONE',  ( -0.3120000000000000551, 0.2090277776260448528, 0.1292346314604056190 ) ) ;
#10641 = VERTEX_POINT ( 'NONE', #5866 ) ;
#10642 = CARTESIAN_POINT ( 'NONE',  ( 0.2819296736111110424, 0.3305555554796889561, -0.1167790944451423119 ) ) ;
#10643 = EDGE_LOOP ( 'NONE', ( #8313, #22144, #5235, #3635 ) ) ;
#10644 = CARTESIAN_POINT ( 'NONE',  ( 0.000000000000000000, 6.000000000000000888, -0.2499999999999999722 ) ) ;
#10645 = DIRECTION ( 'NONE',  ( -0.8459207832372988012, -0.4883925919151527184, -0.2142211582677917836 ) ) ;
#10646 = DIRECTION ( 'NONE',  ( 0.3535533905932763954, -0.7071067811865482389, -0.6123724356957921389 ) ) ;
#10647 = CARTESIAN_POINT ( 'NONE',  ( 0.1116596296178199027, 0.4080357141881718608, 0.3436530038418508792 ) ) ;
#10648 = CARTESIAN_POINT ( 'NONE',  ( -0.04107592630348370910, 5.070398228275294628, 0.3098506894142968870 ) ) ;
#10649 = ADVANCED_FACE ( 'NONE', ( #13216 ), #13325, .T. ) ;
#10650 = FACE_OUTER_BOUND ( 'NONE', #14958, .T. ) ;
#10651 = CARTESIAN_POINT ( 'NONE',  ( -0.08227930641062801420, 3.879488480284497331, -0.3012013832029319382 ) ) ;
#10652 = FACE_OUTER_BOUND ( 'NONE', #15648, .T. ) ;
#10653 = CARTESIAN_POINT ( 'NONE',  ( -0.2819296736111110424, 4.474388888964755395, -0.1167790944451423119 ) ) ;
#10654 = CARTESIAN_POINT ( 'NONE',  ( 0.2772880126055080052, 4.534207701474789687, -0.1455781163606088280 ) ) ;
#10655 = CARTESIAN_POINT ( 'NONE',  ( 0.1993543840281267465, 5.220916666742532186, 0.1993543840281266633 ) ) ;
#10656 = CARTESIAN_POINT ( 'NONE',  ( 0.4687500000000002776, 0.2598076211353318454, 0.06112444011295372487 ) ) ;
#10657 = CARTESIAN_POINT ( 'NONE',  ( 1.201146141948970407E-06, 4.904991752689871198, 0.3119999999951060254 ) ) ;
#10658 = CARTESIAN_POINT ( 'NONE',  ( 0.000000000000000000, 5.580000000000000959, 0.000000000000000000 ) ) ;
#10659 = CARTESIAN_POINT ( 'NONE',  ( -0.05332757804796602052, 4.792349457816412084, 0.3074089561062771647 ) ) ;
#10660 = CARTESIAN_POINT ( 'NONE',  ( 0.2206173157302027954, 4.314666666818398610, -0.2206173157302028232 ) ) ;
#10661 = VECTOR ( 'NONE', #4157, 39.37007874015748143 ) ;
#10662 = CARTESIAN_POINT ( 'NONE',  ( 0.1993543840281266633, 4.790361111186976828, -0.1993543840281266910 ) ) ;
#10663 = CARTESIAN_POINT ( 'NONE',  ( -0.1993543840281266910, 3.734805555631421026, -0.1993543840281266910 ) ) ;
#10664 = ORIENTED_EDGE ( 'NONE', *, *, #16067, .T. ) ;
#10665 = ORIENTED_EDGE ( 'NONE', *, *, #12779, .T. ) ;
#10666 = ADVANCED_FACE ( 'NONE', ( #9783 ), #11252, .T. ) ;
#10667 = EDGE_CURVE ( 'NONE', #5661, #12271, #20626, .T. ) ;
#10668 = EDGE_CURVE ( 'NONE', #19238, #4599, #22694, .T. ) ;
#10669 = ADVANCED_FACE ( 'NONE', ( #7461, #3925 ), #22456, .F. ) ;
#10670 = COORDINATED_UNIVERSAL_TIME_OFFSET ( 0, 0, .AHEAD. ) ;
#10671 = DIRECTION ( 'NONE',  ( 1.000000000000000000, 0.000000000000000000, 0.000000000000000000 ) ) ;
#10672 = CARTESIAN_POINT ( 'NONE',  ( 0.3125000000000000555, -5.740531871003217465E-17, 0.2619444444444478659 ) ) ;
#10673 = VERTEX_POINT ( 'NONE', #19275 ) ;
#10674 = CARTESIAN_POINT ( 'NONE',  ( -5.731347020009612645E-17, 0.2749999998482670627, 0.3119999999999999996 ) ) ;
#10675 = PLANE ( 'NONE',  #826 ) ;
#10676 = CARTESIAN_POINT ( 'NONE',  ( -0.1370262819018738254, 5.125659746303123043, 0.2760471446584434330 ) ) ;
#10677 = VECTOR ( 'NONE', #18413, 39.37007874015748143 ) ;
#10678 = DIRECTION ( 'NONE',  ( 0.8660254037844382635, 0.000000000000000000, 0.5000000000000004441 ) ) ;
#10679 = CARTESIAN_POINT ( 'NONE',  ( -0.2472135954999579999, 0.3749999999999998890, 0.3402603233408160732 ) ) ;
#10680 = EDGE_CURVE ( 'NONE', #5059, #6423, #14115, .T. ) ;
#10681 = ORIENTED_EDGE ( 'NONE', *, *, #5186, .F. ) ;
#10682 = CARTESIAN_POINT ( 'NONE',  ( 0.09537333962189972758, 5.097200745393280386, -0.2967035365653761803 ) ) ;
#10683 = CARTESIAN_POINT ( 'NONE',  ( 0.2819296736111110424, 0.2541666665908000056, 0.1167790944451424923 ) ) ;
#10684 = CARTESIAN_POINT ( 'NONE',  ( -3.385114897866767815E-17, -0.2764156081756484196, 0.3800000000000042233 ) ) ;
#10685 = VERTEX_POINT ( 'NONE', #4521 ) ;
#10686 = CARTESIAN_POINT ( 'NONE',  ( 0.2819296736111110424, 4.550777777853643791, -0.1167790944451423396 ) ) ;
#10687 = CARTESIAN_POINT ( 'NONE',  ( 0.2523926463571754542, 0.1523216146538573512, -0.08381099440924590083 ) ) ;
#10688 = DIRECTION ( 'NONE',  ( 0.000000000000000000, -0.9961946980917454342, -0.08715574274765833240 ) ) ;
#10689 = LINE ( 'NONE', #20432, #18607 ) ;
#10690 = CARTESIAN_POINT ( 'NONE',  ( -0.1292346314604057023, 4.116749999999998799, 0.3119999999999998885 ) ) ;
#10691 = CARTESIAN_POINT ( 'NONE',  ( -0.2206173157302027676, 4.953555555707287894, 0.2206173157302028787 ) ) ;
#10692 = ORIENTED_EDGE ( 'NONE', *, *, #14352, .F. ) ;
#10693 = PLANE ( 'NONE',  #17145 ) ;
#10694 = AXIS2_PLACEMENT_3D ( 'NONE', #10166, #880, #2827 ) ;
#10695 = CARTESIAN_POINT ( 'NONE',  ( -0.1892265952907544457, 4.882961343802892706, -0.2480685101248006896 ) ) ;
#10696 =( BOUNDED_CURVE ( )  B_SPLINE_CURVE ( 2, ( #10506, #16107, #8907, #14277, #17937, #19880, #6961, #16351, #10623, #20124, #18053, #7083, #14522 ),
 .UNSPECIFIED., .F., .F. ) 
 B_SPLINE_CURVE_WITH_KNOTS ( ( 3, 2, 2, 2, 2, 2, 3 ),
 ( 0.3214285714285714524, 0.3285714285714285698, 0.3428571428571428603, 0.3571428571428571508, 0.3714285714285714413, 0.3857142857142857317, 0.3928571428571429047 ),
 .UNSPECIFIED. ) 
 CURVE ( )  GEOMETRIC_REPRESENTATION_ITEM ( )  RATIONAL_B_SPLINE_CURVE ( ( 0.9755282581475767101, 0.9755282581475768211, 1.000000000000000000, 0.9510565162951535312, 1.000000000000000000, 0.9510565162951535312, 1.000000000000000000, 0.9510565162951535312, 1.000000000000000000, 0.9510565162951535312, 1.000000000000000000, 0.9755282581475765991, 0.9755282581475767101 ) ) 
 REPRESENTATION_ITEM ( '' )  );
#10697 = CARTESIAN_POINT ( 'NONE',  ( -0.3155070326520293400, 0.1306872919485614903, 0.3400694444444484765 ) ) ;
#10698 = CARTESIAN_POINT ( 'NONE',  ( 0.2923287055106771337, 0.3616071427596004306, 0.2123892367102621359 ) ) ;
#10699 =( BOUNDED_SURFACE ( )  B_SPLINE_SURFACE ( 1, 2, ( 
 ( #6923, #14485, #1315, #4842, #23609, #19968, #16311, #5199, #5329, #10951, #4962, #19841, #20090, #10590, #12429, #12794, #14361, #21910, #3025, #18017, #18260, #3379, #19722, #8739, #18378, #10472, #1673, #16195, #21791, #1196, #8628, #1555, #16073, #5080, #8993, #16436, #12548, #3255, #23846, #10706, #18141, #1438, #7166, #14609, #15942, #23724, #23368, #8870, #6677, #7049, #14122, #12308, #17902, #23485, #6801, #7766, #15209, #17032, #4101, #9358, #2039, #14859, #7288, #20452, #22276, #16800, #5571, #81, #3619, #13390, #20330, #13275, #16675, #1792, #20693, #11561, #3870, #9106, #9478, #5696, #326, #22644, #18621, #16911, #13159, #5930, #18498, #20812, #16555, #18988, #22518, #14739, #12919, #20573, #14973, #3748, #23977, #11312, #22154, #5451, #11069, #1914, #13036, #206, #11192, #18744, #9235, #24099, #7408, #7526, #22395, #7647, #15095, #5811, #3983, #11434, #18865, #2167, #9600, #14311, #17278, #15567, #21622, #22759, #17971, #3094, #17396, #6744, #22875, #9967, #10539, #8578, #1142, #10091, #1262, #13746, #8690, #22989, #11792, #13633, #23555, #17158, #6294, #16139, #6868, #21746, #5031, #2524, #19345, #8000, #448, #21051, #15452, #689, #6170, #8113, #20933, #12499, #13517, #14188, #9847, #19101, #4916, #2287, #21171, #9722, #2642, #4461, #7879, #15330, #19217, #17511, #11925, #6050, #11678, #4225, #2407, #564, #16018, #4341, #23435, #12378, #19795, #14556, #9299, #22100, #19920, #14918, #16739, #12743, #23795, #11019, #7117, #14683, #11137, #1855, #22, #1384, #22337, #12861, #20280, #21979, #7236, #5273, #5640, #23917, #10897, #7469, #10782, #9057, #14803, #16262, #18567, #20399, #18327, #24042, #16387, #18443, #20157, #8814, #3446, #5396, #3565, #9180, #3206, #10653, #18207, #1623, #16622, #16504, #1503, #18084, #1739, #7352, #6993, #22220, #5519, #12982, #23674, #8938, #14437, #21862, #5152, #3690, #12617, #20035, #3324, #9793, #13223, #22588, #19051, #507, #5873, #18935, #2352, #390, #11377, #3935, #4046, #7829, #17226, #17102, #7940, #15274, #15395, #11500, #11258, #13334, #22938, #270, #22822, #9664, #4287, #20756, #18805, #7709, #2100, #146, #6113, #20875, #13105, #3815, #13581, #4169, #9541, #22702, #5992, #16974, #13457, #15513, #7589, #15156, #11619, #1986, #15040, #2232, #20992, #11744, #19165, #2473, #9908, #17340, #633, #8064, #20633, #20518, #18684, #9422, #16861, #22463, #5762, #4407, #17458, #21359, #6716, #1112, #3062, #15754, #4759, #15634, #12114, #11871, #23166, #19284, #10398, #6478, #6597, #16110, #13929, #990, #8545, #6359, #10155, #19524, #2817, #6234, #2590, #4647, #12231, #23051, #10273, #17821, #14045, #21476, #21242, #11993, #17698, #17580, #10036, #13700, #8419, #869, #15867, #23283, #19641, #2940, #19406, #15987, #23408, #8302, #14161, #21591, #4884, #12349, #13806, #2704, #19766, #10510, #17940, #1236, #8661, #4530, #21117, #751, #8179, #14526, #14280, #20367, #18056, #10748, #11105, #1710, #3177, #18298, #7203, #14775, #8783, #3658, #23523, #22190, #12831, #5001, #10627, #10869, #5241, #18180, #12955, #1596, #6840, #18535, #1825, #16354, #3294, #14649, #1473, #9031, #5489, #9270, #21718, #12463, #19885, #16474, #23885, #8910, #22070, #23765, #1352, #3419, #21948, #16235, #14405, #12713, #18416, #23645, #6964, #24014, #20127, #3538, #20008, #5366, #7086, #21829, #20250, #10991, #9149, #16592, #5120, #12585, #7324, #20605, #13423 ),
 ( #7799, #7558, #22431, #5845, #3902, #14889, #24127, #2070, #11347, #15128, #22554, #11469, #2202, #5732, #4019, #5961, #18774, #358, #22672, #11592, #4135, #9393, #13191, #9511, #7910, #15242, #18902, #11710, #16833, #19133, #15362, #9755, #7678, #7442, #13551, #11226, #16944, #4259, #19023, #20486, #9635, #20845, #15011, #13308, #17065, #2318, #20723, #17192, #478, #22791, #6084, #22308, #243, #2437, #20965, #16710, #5606, #13071, #3782, #18654, #1947, #116, #8270, #15719, #4616, #19491, #15601, #21327, #23252, #11961, #17666, #15833, #4729, #21443, #2557, #23024, #21204, #1078, #8383, #12079, #4849, #10004, #12317, #8509, #2903, #841, #601, #6684, #4374, #4496, #21558, #12201, #13670, #2785, #952, #721, #23133, #10238, #6562, #13898, #14012, #19608, #10362, #6446, #8032, #2673, #19729, #19376, #17785, #15950, #23376, #17548, #8149, #10123, #6325, #21084, #14129, #9879, #17308, #15483, #22909, #6204, #13777, #11832, #19251, #17428, #3387, #5461, #21685, #18025, #5208, #16080, #4968, #8747, #7056, #14368, #21800, #6931, #20099, #9000, #18149, #5087, #10597, #12681, #10840, #16564, #22162, #1443, #6808, #1204, #14250, #8877, #3509, #22042, #23986, #12554, #1564, #12435, #16319, #8635, #19976, #23492, #7174, #3263, #18268, #12927, #10714, #21916, #5337, #3147, #23731, #14493, #16444, #3032, #19849, #23855, #14617, #1322, #12802, #20221, #10961, #18386, #16203, #23616, #1681, #9114, #7297, #14747, #10479, #17909, #15219, #333, #24106, #18629, #22766, #7416, #9729, #7532, #16808, #5578, #13043, #17039, #20460, #5704, #2175, #7773, #13166, #2047, #9609, #7654, #1922, #3877, #20820, #22651, #18874, #3991, #11569, #15102, #2294, #16918, #20580, #14981, #17167, #11077, #9486, #18996, #455, #4110, #15338, #11320, #13283, #9366, #18507, #22403, #88, #18751, #215, #22526, #14867, #7886, #22283, #5939, #3757, #11199, #13397, #6058, #5818, #20339, #20701, #11442, #3627, #1799, #9243, #16685, #10098, #4706, #22882, #10334, #13526, #12174, #2763, #19109, #17284, #814, #19351, #8123, #2875, #15695, #20940, #8482, #17761, #6301, #17403, #4593, #696, #8241, #19582, #1055, #15924, #2413, #23347, #6418, #13872, #15574, #23109, #22997, #4233, #17519, #4468, #11685, #4348, #2648, #8359, #9855, #572, #13989, #11932, #17640, #9976, #12052, #13754, #8007, #21179, #21300, #19465, #10214, #15459, #6177, #11802, #929, #15809, #23228, #19224, #13641, #6537, #21059, #2531, #21417, #23830, #21777, #21534, #3483, #1176, #18006, #18362, #8973, #10457, #1422, #14472, #21659, #5063, #18124, #3363, #10690, #10815, #8850, #18242, #12533, #4821, #23589, #16540, #1298, #1541, #3242, #22015, #14344, #4947, #8723, #12411, #17884, #16421, #21896, #6658, #12291, #7152, #5185, #19830, #16296, #23709, #3125, #7031, #9090, #8614, #10576, #12656, #19705, #16055, #16176, #20074, #6906, #19952, #14592, #5313, #12776, #20195, #10934, #14223, #1655, #14105, #3007, #23470, #6781, #3600, #22134, #11052, #14954, #303, #18842, #20788, #9339, #22496, #9219, #5675, #5435, #16775, #12900, #3965, #60, #183, #9698, #7506, #18721, #2139, #24080, #3729, #13140, #20553, #23958, #20316, #22374, #5791, #16658, #3848, #11409, #7623, #15074, #14840, #5553, #11293, #11176, #18481, #7272, #2020, #18603, #9457, #16890, #13255, #20672, #13018, #9577, #17010, #1896, #7743, #15187, #22624, #5910, #7388, #20433, #13367, #4079, #11534 ) ),
 .UNSPECIFIED., .F., .F., .F. ) 
 B_SPLINE_SURFACE_WITH_KNOTS ( ( 2, 2 ),
 ( 3, 2, 2, 2, 2, 2, 2, 2, 2, 2, 2, 2, 2, 2, 2, 2, 2, 2, 2, 2, 2, 2, 2, 2, 2, 2, 2, 2, 2, 2, 2, 2, 2, 2, 2, 2, 2, 2, 2, 2, 2, 2, 2, 2, 2, 2, 2, 2, 2, 2, 2, 2, 2, 2, 2, 2, 2, 2, 2, 2, 2, 2, 2, 2, 2, 2, 2, 2, 2, 2, 2, 2, 2, 2, 2, 2, 2, 2, 2, 2, 2, 2, 2, 2, 2, 2, 2, 2, 2, 2, 2, 2, 2, 2, 2, 2, 2, 2, 2, 2, 2, 2, 2, 2, 2, 2, 2, 2, 2, 2, 2, 2, 2, 2, 2, 2, 2, 2, 2, 2, 2, 2, 2, 2, 2, 2, 2, 2, 2, 2, 2, 2, 2, 2, 2, 2, 2, 2, 2, 2, 2, 2, 2, 2, 2, 2, 2, 2, 2, 2, 2, 2, 2, 2, 2, 2, 2, 2, 2, 2, 2, 2, 2, 2, 2, 2, 2, 2, 2, 2, 2, 2, 2, 2, 2, 2, 2, 2, 2, 2, 2, 2, 2, 2, 2, 2, 2, 2, 2, 2, 2, 2, 2, 2, 2, 2, 2, 2, 2, 2, 2, 2, 2, 2, 2, 2, 2, 2, 2, 2, 2, 2, 2, 2, 2, 2, 2, 2, 2, 2, 3 ),
 ( 0.000000000000000000, 1.000000000000000000 ),
 ( 0.000000000000000000, 0.004464285714285714038, 0.008928571428571428076, 0.01339285714285714211, 0.01785714285714285615, 0.02232142857142857192, 0.02678571428571428423, 0.03125000000000000000, 0.03571428571428571230, 0.04017857142857143155, 0.04464285714285714385, 0.04910714285714285615, 0.05357142857142856845, 0.05803571428571428770, 0.06250000000000000000, 0.06696428571428571230, 0.07142857142857142461, 0.07589285714285713691, 0.08035714285714286309, 0.08482142857142857539, 0.08928571428571428770, 0.09375000000000000000, 0.09821428571428571230, 0.1026785714285714246, 0.1071428571428571369, 0.1116071428571428631, 0.1160714285714285754, 0.1205357142857142877, 0.1250000000000000000, 0.1294642857142857262, 0.1339285714285714246, 0.1383928571428571508, 0.1428571428571428492, 0.1473214285714285754, 0.1517857142857142738, 0.1562500000000000000, 0.1607142857142857262, 0.1651785714285714246, 0.1696428571428571508, 0.1741071428571428492, 0.1785714285714285754, 0.1830357142857142738, 0.1875000000000000000, 0.1919642857142857262, 0.1964285714285714246, 0.2008928571428571508, 0.2053571428571428492, 0.2098214285714285754, 0.2142857142857142738, 0.2187500000000000000, 0.2232142857142857262, 0.2276785714285714246, 0.2321428571428571508, 0.2366071428571428492, 0.2410714285714285754, 0.2455357142857142738, 0.2500000000000000000, 0.2544642857142856984, 0.2589285714285714524, 0.2633928571428571508, 0.2678571428571428492, 0.2723214285714285476, 0.2767857142857143016, 0.2812500000000000000, 0.2857142857142856984, 0.2901785714285714524, 0.2946428571428571508, 0.2991071428571428492, 0.3035714285714285476, 0.3080357142857143016, 0.3125000000000000000, 0.3169642857142856984, 0.3214285714285714524, 0.3258928571428571508, 0.3303571428571428492, 0.3348214285714285476, 0.3392857142857143016, 0.3437500000000000000, 0.3482142857142856984, 0.3526785714285714524, 0.3571428571428571508, 0.3616071428571428492, 0.3660714285714285476, 0.3705357142857143016, 0.3750000000000000000, 0.3794642857142856984, 0.3839285714285714524, 0.3883928571428571508, 0.3928571428571428492, 0.3973214285714285476, 0.4017857142857143016, 0.4062500000000000000, 0.4107142857142856984, 0.4151785714285714524, 0.4196428571428571508, 0.4241071428571428492, 0.4285714285714285476, 0.4330357142857143016, 0.4375000000000000000, 0.4419642857142856984, 0.4464285714285714524, 0.4508928571428571508, 0.4553571428571428492, 0.4598214285714285476, 0.4642857142857143016, 0.4687500000000000000, 0.4732142857142856984, 0.4776785714285714524, 0.4821428571428571508, 0.4866071428571428492, 0.4910714285714285476, 0.4955357142857143016, 0.5000000000000000000, 0.5044642857142856984, 0.5089285714285713969, 0.5133928571428570953, 0.5178571428571429047, 0.5223214285714286031, 0.5267857142857143016, 0.5312500000000000000, 0.5357142857142856984, 0.5401785714285713969, 0.5446428571428570953, 0.5491071428571429047, 0.5535714285714286031, 0.5580357142857143016, 0.5625000000000000000, 0.5669642857142856984, 0.5714285714285713969, 0.5758928571428570953, 0.5803571428571429047, 0.5848214285714286031, 0.5892857142857143016, 0.5937500000000000000, 0.5982142857142856984, 0.6026785714285713969, 0.6071428571428570953, 0.6116071428571429047, 0.6160714285714286031, 0.6205357142857143016, 0.6250000000000000000, 0.6294642857142856984, 0.6339285714285713969, 0.6383928571428570953, 0.6428571428571429047, 0.6473214285714286031, 0.6517857142857143016, 0.6562500000000000000, 0.6607142857142856984, 0.6651785714285713969, 0.6696428571428570953, 0.6741071428571429047, 0.6785714285714286031, 0.6830357142857143016, 0.6875000000000000000, 0.6919642857142856984, 0.6964285714285713969, 0.7008928571428570953, 0.7053571428571429047, 0.7098214285714286031, 0.7142857142857143016, 0.7187500000000000000, 0.7232142857142856984, 0.7276785714285713969, 0.7321428571428570953, 0.7366071428571429047, 0.7410714285714286031, 0.7455357142857143016, 0.7500000000000000000, 0.7544642857142856984, 0.7589285714285713969, 0.7633928571428570953, 0.7678571428571429047, 0.7723214285714286031, 0.7767857142857143016, 0.7812500000000000000, 0.7857142857142856984, 0.7901785714285713969, 0.7946428571428570953, 0.7991071428571429047, 0.8035714285714286031, 0.8080357142857143016, 0.8125000000000000000, 0.8169642857142856984, 0.8214285714285713969, 0.8258928571428570953, 0.8303571428571429047, 0.8348214285714286031, 0.8392857142857143016, 0.8437500000000000000, 0.8482142857142856984, 0.8526785714285713969, 0.8571428571428570953, 0.8616071428571429047, 0.8660714285714286031, 0.8705357142857143016, 0.8750000000000000000, 0.8794642857142856984, 0.8839285714285713969, 0.8883928571428570953, 0.8928571428571429047, 0.8973214285714286031, 0.9017857142857143016, 0.9062500000000000000, 0.9107142857142856984, 0.9151785714285713969, 0.9196428571428570953, 0.9241071428571429047, 0.9285714285714286031, 0.9330357142857143016, 0.9375000000000000000, 0.9419642857142856984, 0.9464285714285713969, 0.9508928571428570953, 0.9553571428571429047, 0.9598214285714286031, 0.9642857142857143016, 0.9687500000000000000, 0.9732142857142856984, 0.9771335280684947389, 0.9869048633491797062 ),
 .UNSPECIFIED. ) 
 GEOMETRIC_REPRESENTATION_ITEM ( )  RATIONAL_B_SPLINE_SURFACE ( (
 ( 1.000000000000000000, 0.9238795325112867385, 1.000000000000000000, 0.9238795325112867385, 1.000000000000000000, 0.9238795325112867385, 1.000000000000000000, 0.9238795325112867385, 1.000000000000000000, 0.9238795325112867385, 1.000000000000000000, 0.9238795325112867385, 1.000000000000000000, 0.9238795325112867385, 1.000000000000000000, 0.9238795325112867385, 1.000000000000000000, 0.9238795325112867385, 1.000000000000000000, 0.9238795325112867385, 1.000000000000000000, 0.9238795325112867385, 1.000000000000000000, 0.9238795325112867385, 1.000000000000000000, 0.9238795325112867385, 1.000000000000000000, 0.9238795325112867385, 1.000000000000000000, 0.9238795325112867385, 1.000000000000000000, 0.9238795325112867385, 1.000000000000000000, 0.9238795325112867385, 1.000000000000000000, 0.9238795325112867385, 1.000000000000000000, 0.9238795325112867385, 1.000000000000000000, 0.9238795325112867385, 1.000000000000000000, 0.9238795325112867385, 1.000000000000000000, 0.9238795325112867385, 1.000000000000000000, 0.9238795325112867385, 1.000000000000000000, 0.9238795325112867385, 1.000000000000000000, 0.9238795325112867385, 1.000000000000000000, 0.9238795325112867385, 1.000000000000000000, 0.9238795325112867385, 1.000000000000000000, 0.9238795325112867385, 1.000000000000000000, 0.9238795325112867385, 1.000000000000000000, 0.9238795325112867385, 1.000000000000000000, 0.9238795325112867385, 1.000000000000000000, 0.9238795325112867385, 1.000000000000000000, 0.9238795325112867385, 1.000000000000000000, 0.9238795325112867385, 1.000000000000000000, 0.9238795325112867385, 1.000000000000000000, 0.9238795325112867385, 1.000000000000000000, 0.9238795325112867385, 1.000000000000000000, 0.9238795325112867385, 1.000000000000000000, 0.9238795325112867385, 1.000000000000000000, 0.9238795325112867385, 1.000000000000000000, 0.9238795325112867385, 1.000000000000000000, 0.9238795325112867385, 1.000000000000000000, 0.9238795325112867385, 1.000000000000000000, 0.9238795325112867385, 1.000000000000000000, 0.9238795325112867385, 1.000000000000000000, 0.9238795325112867385, 1.000000000000000000, 0.9238795325112867385, 1.000000000000000000, 0.9238795325112867385, 1.000000000000000000, 0.9238795325112867385, 1.000000000000000000, 0.9238795325112867385, 1.000000000000000000, 0.9238795325112867385, 1.000000000000000000, 0.9238795325112867385, 1.000000000000000000, 0.9238795325112867385, 1.000000000000000000, 0.9238795325112867385, 1.000000000000000000, 0.9238795325112867385, 1.000000000000000000, 0.9238795325112867385, 1.000000000000000000, 0.9238795325112867385, 1.000000000000000000, 0.9238795325112867385, 1.000000000000000000, 0.9238795325112867385, 1.000000000000000000, 0.9238795325112867385, 1.000000000000000000, 0.9238795325112867385, 1.000000000000000000, 0.9238795325112867385, 1.000000000000000000, 0.9238795325112867385, 1.000000000000000000, 0.9238795325112867385, 1.000000000000000000, 0.9238795325112867385, 1.000000000000000000, 0.9238795325112867385, 1.000000000000000000, 0.9238795325112867385, 1.000000000000000000, 0.9238795325112867385, 1.000000000000000000, 0.9238795325112867385, 1.000000000000000000, 0.9238795325112867385, 1.000000000000000000, 0.9238795325112867385, 1.000000000000000000, 0.9238795325112867385, 1.000000000000000000, 0.9238795325112867385, 1.000000000000000000, 0.9238795325112867385, 1.000000000000000000, 0.9238795325112867385, 1.000000000000000000, 0.9238795325112867385, 1.000000000000000000, 0.9238795325112867385, 1.000000000000000000, 0.9238795325112867385, 1.000000000000000000, 0.9238795325112867385, 1.000000000000000000, 0.9238795325112867385, 1.000000000000000000, 0.9238795325112867385, 1.000000000000000000, 0.9238795325112867385, 1.000000000000000000, 0.9238795325112867385, 1.000000000000000000, 0.9238795325112867385, 1.000000000000000000, 0.9238795325112867385, 1.000000000000000000, 0.9238795325112867385, 1.000000000000000000, 0.9238795325112867385, 1.000000000000000000, 0.9238795325112867385, 1.000000000000000000, 0.9238795325112867385, 1.000000000000000000, 0.9238795325112867385, 1.000000000000000000, 0.9238795325112867385, 1.000000000000000000, 0.9238795325112867385, 1.000000000000000000, 0.9238795325112867385, 1.000000000000000000, 0.9238795325112867385, 1.000000000000000000, 0.9238795325112867385, 1.000000000000000000, 0.9238795325112867385, 1.000000000000000000, 0.9238795325112867385, 1.000000000000000000, 0.9238795325112867385, 1.000000000000000000, 0.9238795325112867385, 1.000000000000000000, 0.9238795325112867385, 1.000000000000000000, 0.9238795325112867385, 1.000000000000000000, 0.9238795325112867385, 1.000000000000000000, 0.9238795325112867385, 1.000000000000000000, 0.9238795325112867385, 1.000000000000000000, 0.9238795325112867385, 1.000000000000000000, 0.9238795325112867385, 1.000000000000000000, 0.9238795325112867385, 1.000000000000000000, 0.9238795325112867385, 1.000000000000000000, 0.9238795325112867385, 1.000000000000000000, 0.9238795325112867385, 1.000000000000000000, 0.9238795325112867385, 1.000000000000000000, 0.9238795325112867385, 1.000000000000000000, 0.9238795325112867385, 1.000000000000000000, 0.9238795325112867385, 1.000000000000000000, 0.9238795325112867385, 1.000000000000000000, 0.9238795325112867385, 1.000000000000000000, 0.9238795325112867385, 1.000000000000000000, 0.9238795325112867385, 1.000000000000000000, 0.9238795325112867385, 1.000000000000000000, 0.9238795325112867385, 1.000000000000000000, 0.9238795325112867385, 1.000000000000000000, 0.9238795325112867385, 1.000000000000000000, 0.9238795325112867385, 1.000000000000000000, 0.9238795325112867385, 1.000000000000000000, 0.9238795325112867385, 1.000000000000000000, 0.9238795325112867385, 1.000000000000000000, 0.9238795325112867385, 1.000000000000000000, 0.9238795325112867385, 1.000000000000000000, 0.9238795325112867385, 1.000000000000000000, 0.9238795325112867385, 1.000000000000000000, 0.9238795325112867385, 1.000000000000000000, 0.9238795325112867385, 1.000000000000000000, 0.9238795325112867385, 1.000000000000000000, 0.9238795325112867385, 1.000000000000000000, 0.9238795325112867385, 1.000000000000000000, 0.9238795325112867385, 1.000000000000000000, 0.9238795325112867385, 1.000000000000000000, 0.9238795325112867385, 1.000000000000000000, 0.9238795325112867385, 1.000000000000000000, 0.9238795325112867385, 1.000000000000000000, 0.9238795325112867385, 1.000000000000000000, 0.9238795325112867385, 1.000000000000000000, 0.9238795325112867385, 1.000000000000000000, 0.9238795325112867385, 1.000000000000000000, 0.9238795325112867385, 1.000000000000000000, 0.9238795325112867385, 1.000000000000000000, 0.9238795325112867385, 1.000000000000000000, 0.9238795325112867385, 1.000000000000000000, 0.9238795325112867385, 1.000000000000000000, 0.9238795325112867385, 1.000000000000000000, 0.9238795325112867385, 1.000000000000000000, 0.9238795325112867385, 1.000000000000000000, 0.9238795325112867385, 1.000000000000000000, 0.9238795325112867385, 1.000000000000000000, 0.9238795325112867385, 1.000000000000000000, 0.9238795325112867385, 1.000000000000000000, 0.9238795325112867385, 1.000000000000000000, 0.9238795325112867385, 1.000000000000000000, 0.9238795325112867385, 1.000000000000000000, 0.9238795325112867385, 1.000000000000000000, 0.9238795325112867385, 1.000000000000000000, 0.9238795325112867385, 1.000000000000000000, 0.9238795325112867385, 1.000000000000000000, 0.9238795325112867385, 1.000000000000000000, 0.9238795325112867385, 1.000000000000000000, 0.9238795325112867385, 1.000000000000000000, 0.9238795325112867385, 1.000000000000000000, 0.9238795325112867385, 1.000000000000000000, 0.9238795325112867385, 1.000000000000000000, 0.9238795325112867385, 1.000000000000000000, 0.9238795325112867385, 1.000000000000000000, 0.9238795325112867385, 1.000000000000000000, 0.9238795325112867385, 1.000000000000000000, 0.9238795325112867385, 1.000000000000000000, 0.9238795325112867385, 1.000000000000000000, 0.9238795325112867385, 1.000000000000000000, 0.9238795325112867385, 1.000000000000000000, 0.9238795325112867385, 1.000000000000000000, 0.9238795325112867385, 1.000000000000000000, 0.9238795325112867385, 1.000000000000000000, 0.9238795325112867385, 1.000000000000000000, 0.9238795325112867385, 1.000000000000000000, 0.9238795325112867385, 1.000000000000000000, 0.9238795325112867385, 1.000000000000000000, 0.9238795325112867385, 1.000000000000000000, 0.9238795325112867385, 1.000000000000000000, 0.9238795325112867385, 1.000000000000000000, 0.9238795325112867385, 1.000000000000000000, 0.9238795325112867385, 1.000000000000000000, 0.9238795325112867385, 1.000000000000000000, 0.9238795325112867385, 1.000000000000000000, 0.9238795325112867385, 1.000000000000000000, 0.9238795325112867385, 1.000000000000000000, 0.9238795325112867385, 1.000000000000000000, 0.9238795325112867385, 1.000000000000000000, 0.9238795325112867385, 1.000000000000000000, 0.9238795325112867385, 1.000000000000000000, 0.9238795325112867385, 1.000000000000000000, 0.9238795325112867385, 1.000000000000000000, 0.9238795325112867385, 1.000000000000000000, 0.9238795325112867385, 1.000000000000000000, 0.9238795325112867385, 1.000000000000000000, 0.9238795325112867385, 1.000000000000000000, 0.9238795325112867385, 1.000000000000000000, 0.9238795325112867385, 1.000000000000000000, 0.9238795325112867385, 1.000000000000000000, 0.9238795325112867385, 1.000000000000000000, 0.9238795325112867385, 1.000000000000000000, 0.9238795325112867385, 1.000000000000000000, 0.9238795325112867385, 1.000000000000000000, 0.9238795325112867385, 1.000000000000000000, 0.9238795325112867385, 1.000000000000000000, 0.9238795325112867385, 1.000000000000000000, 0.9238795325112867385, 1.000000000000000000, 0.9238795325112867385, 1.000000000000000000, 0.9238795325112867385, 1.000000000000000000, 0.9238795325112867385, 1.000000000000000000, 0.9238795325112867385, 1.000000000000000000, 0.9331730585143133139, 0.9836822358325096882, 0.9836822358325096882, 0.9836822358325096882),
 ( 1.000000000000000000, 0.9238795325112867385, 1.000000000000000000, 0.9238795325112867385, 1.000000000000000000, 0.9238795325112867385, 1.000000000000000000, 0.9238795325112867385, 1.000000000000000000, 0.9238795325112867385, 1.000000000000000000, 0.9238795325112867385, 1.000000000000000000, 0.9238795325112867385, 1.000000000000000000, 0.9238795325112867385, 1.000000000000000000, 0.9238795325112867385, 1.000000000000000000, 0.9238795325112867385, 1.000000000000000000, 0.9238795325112867385, 1.000000000000000000, 0.9238795325112867385, 1.000000000000000000, 0.9238795325112867385, 1.000000000000000000, 0.9238795325112867385, 1.000000000000000000, 0.9238795325112867385, 1.000000000000000000, 0.9238795325112867385, 1.000000000000000000, 0.9238795325112867385, 1.000000000000000000, 0.9238795325112867385, 1.000000000000000000, 0.9238795325112867385, 1.000000000000000000, 0.9238795325112867385, 1.000000000000000000, 0.9238795325112867385, 1.000000000000000000, 0.9238795325112867385, 1.000000000000000000, 0.9238795325112867385, 1.000000000000000000, 0.9238795325112867385, 1.000000000000000000, 0.9238795325112867385, 1.000000000000000000, 0.9238795325112867385, 1.000000000000000000, 0.9238795325112867385, 1.000000000000000000, 0.9238795325112867385, 1.000000000000000000, 0.9238795325112867385, 1.000000000000000000, 0.9238795325112867385, 1.000000000000000000, 0.9238795325112867385, 1.000000000000000000, 0.9238795325112867385, 1.000000000000000000, 0.9238795325112867385, 1.000000000000000000, 0.9238795325112867385, 1.000000000000000000, 0.9238795325112867385, 1.000000000000000000, 0.9238795325112867385, 1.000000000000000000, 0.9238795325112867385, 1.000000000000000000, 0.9238795325112867385, 1.000000000000000000, 0.9238795325112867385, 1.000000000000000000, 0.9238795325112867385, 1.000000000000000000, 0.9238795325112867385, 1.000000000000000000, 0.9238795325112867385, 1.000000000000000000, 0.9238795325112867385, 1.000000000000000000, 0.9238795325112867385, 1.000000000000000000, 0.9238795325112867385, 1.000000000000000000, 0.9238795325112867385, 1.000000000000000000, 0.9238795325112867385, 1.000000000000000000, 0.9238795325112867385, 1.000000000000000000, 0.9238795325112867385, 1.000000000000000000, 0.9238795325112867385, 1.000000000000000000, 0.9238795325112867385, 1.000000000000000000, 0.9238795325112867385, 1.000000000000000000, 0.9238795325112867385, 1.000000000000000000, 0.9238795325112867385, 1.000000000000000000, 0.9238795325112867385, 1.000000000000000000, 0.9238795325112867385, 1.000000000000000000, 0.9238795325112867385, 1.000000000000000000, 0.9238795325112867385, 1.000000000000000000, 0.9238795325112867385, 1.000000000000000000, 0.9238795325112867385, 1.000000000000000000, 0.9238795325112867385, 1.000000000000000000, 0.9238795325112867385, 1.000000000000000000, 0.9238795325112867385, 1.000000000000000000, 0.9238795325112867385, 1.000000000000000000, 0.9238795325112867385, 1.000000000000000000, 0.9238795325112867385, 1.000000000000000000, 0.9238795325112867385, 1.000000000000000000, 0.9238795325112867385, 1.000000000000000000, 0.9238795325112867385, 1.000000000000000000, 0.9238795325112867385, 1.000000000000000000, 0.9238795325112867385, 1.000000000000000000, 0.9238795325112867385, 1.000000000000000000, 0.9238795325112867385, 1.000000000000000000, 0.9238795325112867385, 1.000000000000000000, 0.9238795325112867385, 1.000000000000000000, 0.9238795325112867385, 1.000000000000000000, 0.9238795325112867385, 1.000000000000000000, 0.9238795325112867385, 1.000000000000000000, 0.9238795325112867385, 1.000000000000000000, 0.9238795325112867385, 1.000000000000000000, 0.9238795325112867385, 1.000000000000000000, 0.9238795325112867385, 1.000000000000000000, 0.9238795325112867385, 1.000000000000000000, 0.9238795325112867385, 1.000000000000000000, 0.9238795325112867385, 1.000000000000000000, 0.9238795325112867385, 1.000000000000000000, 0.9238795325112867385, 1.000000000000000000, 0.9238795325112867385, 1.000000000000000000, 0.9238795325112867385, 1.000000000000000000, 0.9238795325112867385, 1.000000000000000000, 0.9238795325112867385, 1.000000000000000000, 0.9238795325112867385, 1.000000000000000000, 0.9238795325112867385, 1.000000000000000000, 0.9238795325112867385, 1.000000000000000000, 0.9238795325112867385, 1.000000000000000000, 0.9238795325112867385, 1.000000000000000000, 0.9238795325112867385, 1.000000000000000000, 0.9238795325112867385, 1.000000000000000000, 0.9238795325112867385, 1.000000000000000000, 0.9238795325112867385, 1.000000000000000000, 0.9238795325112867385, 1.000000000000000000, 0.9238795325112867385, 1.000000000000000000, 0.9238795325112867385, 1.000000000000000000, 0.9238795325112867385, 1.000000000000000000, 0.9238795325112867385, 1.000000000000000000, 0.9238795325112867385, 1.000000000000000000, 0.9238795325112867385, 1.000000000000000000, 0.9238795325112867385, 1.000000000000000000, 0.9238795325112867385, 1.000000000000000000, 0.9238795325112867385, 1.000000000000000000, 0.9238795325112867385, 1.000000000000000000, 0.9238795325112867385, 1.000000000000000000, 0.9238795325112867385, 1.000000000000000000, 0.9238795325112867385, 1.000000000000000000, 0.9238795325112867385, 1.000000000000000000, 0.9238795325112867385, 1.000000000000000000, 0.9238795325112867385, 1.000000000000000000, 0.9238795325112867385, 1.000000000000000000, 0.9238795325112867385, 1.000000000000000000, 0.9238795325112867385, 1.000000000000000000, 0.9238795325112867385, 1.000000000000000000, 0.9238795325112867385, 1.000000000000000000, 0.9238795325112867385, 1.000000000000000000, 0.9238795325112867385, 1.000000000000000000, 0.9238795325112867385, 1.000000000000000000, 0.9238795325112867385, 1.000000000000000000, 0.9238795325112867385, 1.000000000000000000, 0.9238795325112867385, 1.000000000000000000, 0.9238795325112867385, 1.000000000000000000, 0.9238795325112867385, 1.000000000000000000, 0.9238795325112867385, 1.000000000000000000, 0.9238795325112867385, 1.000000000000000000, 0.9238795325112867385, 1.000000000000000000, 0.9238795325112867385, 1.000000000000000000, 0.9238795325112867385, 1.000000000000000000, 0.9238795325112867385, 1.000000000000000000, 0.9238795325112867385, 1.000000000000000000, 0.9238795325112867385, 1.000000000000000000, 0.9238795325112867385, 1.000000000000000000, 0.9238795325112867385, 1.000000000000000000, 0.9238795325112867385, 1.000000000000000000, 0.9238795325112867385, 1.000000000000000000, 0.9238795325112867385, 1.000000000000000000, 0.9238795325112867385, 1.000000000000000000, 0.9238795325112867385, 1.000000000000000000, 0.9238795325112867385, 1.000000000000000000, 0.9238795325112867385, 1.000000000000000000, 0.9238795325112867385, 1.000000000000000000, 0.9238795325112867385, 1.000000000000000000, 0.9238795325112867385, 1.000000000000000000, 0.9238795325112867385, 1.000000000000000000, 0.9238795325112867385, 1.000000000000000000, 0.9238795325112867385, 1.000000000000000000, 0.9238795325112867385, 1.000000000000000000, 0.9238795325112867385, 1.000000000000000000, 0.9238795325112867385, 1.000000000000000000, 0.9238795325112867385, 1.000000000000000000, 0.9238795325112867385, 1.000000000000000000, 0.9238795325112867385, 1.000000000000000000, 0.9238795325112867385, 1.000000000000000000, 0.9238795325112867385, 1.000000000000000000, 0.9238795325112867385, 1.000000000000000000, 0.9238795325112867385, 1.000000000000000000, 0.9238795325112867385, 1.000000000000000000, 0.9238795325112867385, 1.000000000000000000, 0.9238795325112867385, 1.000000000000000000, 0.9238795325112867385, 1.000000000000000000, 0.9238795325112867385, 1.000000000000000000, 0.9238795325112867385, 1.000000000000000000, 0.9238795325112867385, 1.000000000000000000, 0.9238795325112867385, 1.000000000000000000, 0.9238795325112867385, 1.000000000000000000, 0.9238795325112867385, 1.000000000000000000, 0.9238795325112867385, 1.000000000000000000, 0.9238795325112867385, 1.000000000000000000, 0.9238795325112867385, 1.000000000000000000, 0.9238795325112867385, 1.000000000000000000, 0.9238795325112867385, 1.000000000000000000, 0.9238795325112867385, 1.000000000000000000, 0.9238795325112867385, 1.000000000000000000, 0.9238795325112867385, 1.000000000000000000, 0.9238795325112867385, 1.000000000000000000, 0.9238795325112867385, 1.000000000000000000, 0.9238795325112867385, 1.000000000000000000, 0.9238795325112867385, 1.000000000000000000, 0.9238795325112867385, 1.000000000000000000, 0.9238795325112867385, 1.000000000000000000, 0.9238795325112867385, 1.000000000000000000, 0.9238795325112867385, 1.000000000000000000, 0.9238795325112867385, 1.000000000000000000, 0.9238795325112867385, 1.000000000000000000, 0.9238795325112867385, 1.000000000000000000, 0.9238795325112867385, 1.000000000000000000, 0.9238795325112867385, 1.000000000000000000, 0.9238795325112867385, 1.000000000000000000, 0.9238795325112867385, 1.000000000000000000, 0.9238795325112867385, 1.000000000000000000, 0.9238795325112867385, 1.000000000000000000, 0.9238795325112867385, 1.000000000000000000, 0.9238795325112867385, 1.000000000000000000, 0.9238795325112867385, 1.000000000000000000, 0.9238795325112867385, 1.000000000000000000, 0.9238795325112867385, 1.000000000000000000, 0.9238795325112867385, 1.000000000000000000, 0.9238795325112867385, 1.000000000000000000, 0.9238795325112867385, 1.000000000000000000, 0.9238795325112867385, 1.000000000000000000, 0.9238795325112867385, 1.000000000000000000, 0.9238795325112867385, 1.000000000000000000, 0.9238795325112867385, 1.000000000000000000, 0.9238795325112867385, 1.000000000000000000, 0.9238795325112867385, 1.000000000000000000, 0.9238795325112867385, 1.000000000000000000, 0.9238795325112867385, 1.000000000000000000, 0.9238795325112867385, 1.000000000000000000, 0.9238795325112867385, 1.000000000000000000, 0.9238795325112867385, 1.000000000000000000, 0.9238795325112867385, 1.000000000000000000, 0.9331730585143133139, 0.9836822358325096882, 0.9836822358325096882, 0.9836822358325096882) ) ) 
 REPRESENTATION_ITEM ( '' )  SURFACE ( )  );
#10700 = VECTOR ( 'NONE', #11269, 39.37007874015748143 ) ;
#10701 = EDGE_CURVE ( 'NONE', #5752, #12807, #15626, .T. ) ;
#10702 = DIRECTION ( 'NONE',  ( -1.224646799147353207E-16, 1.000000000000000000, 0.000000000000000000 ) ) ;
#10703 = CARTESIAN_POINT ( 'NONE',  ( -0.3613381517857143232, 0.3151785713310290005, -4.425116109941954795E-17 ) ) ;
#10704 = CARTESIAN_POINT ( 'NONE',  ( -0.2819296736111111534, 0.2472222221463555580, 0.1167790944451422563 ) ) ;
#10705 = CARTESIAN_POINT ( 'NONE',  ( 0.2764156081756483641, -0.1144950937579611167, 0.008472222222223456389 ) ) ;
#10706 = CARTESIAN_POINT ( 'NONE',  ( 0.2819296736111110424, 5.120222222298088433, -0.1167790944451423396 ) ) ;
#10707 = DIRECTION ( 'NONE',  ( -0.000000000000000000, -1.000000000000000000, -0.000000000000000000 ) ) ;
#10708 = AXIS2_PLACEMENT_3D ( 'NONE', #5715, #12937, #18515 ) ;
#10709 = ORIENTED_EDGE ( 'NONE', *, *, #2102, .F. ) ;
#10710 = CARTESIAN_POINT ( 'NONE',  ( -1.910449006669871087E-17, 3.870222222222221564, -0.3119999999999999996 ) ) ;
#10711 = CARTESIAN_POINT ( 'NONE',  ( -0.0006126656105341529409, 4.293815956690722579, 0.3119994368665558460 ) ) ;
#10712 = CYLINDRICAL_SURFACE ( 'NONE', #7880, 0.3125000000000000000 ) ;
#10713 = CARTESIAN_POINT ( 'NONE',  ( -0.4801334617939588822, 0.2624565244266455766, 0.04287645741408795813 ) ) ;
#10714 = CARTESIAN_POINT ( 'NONE',  ( 0.2206173157302027954, 4.696611111111110404, -0.2206173157302028232 ) ) ;
#10715 = CARTESIAN_POINT ( 'NONE',  ( 0.1182602959184163444, 5.202871751913769494, 0.2584494713975609703 ) ) ;
#10716 = CARTESIAN_POINT ( 'NONE',  ( -1.726321361862525858E-17, 3.894527777853643347, -0.2819296736111110979 ) ) ;
#10717 = CARTESIAN_POINT ( 'NONE',  ( 0.1167790944451422702, 3.793833333409199149, -0.2819296736111110424 ) ) ;
#10718 = DIRECTION ( 'NONE',  ( 8.659560562355053653E-17, -0.7071067811865376918, 0.7071067811865573427 ) ) ;
#10719 = CC_DESIGN_APPROVAL ( #619, ( #11949 ) ) ;
#10720 = PLANE ( 'NONE',  #10175 ) ;
#10721 = APPROVAL_PERSON_ORGANIZATION ( #6942, #2844, #19861 ) ;
#10722 = ORIENTED_EDGE ( 'NONE', *, *, #21273, .T. ) ;
#10723 = CARTESIAN_POINT ( 'NONE',  ( -3.827021247335479543E-17, -0.3125000000000000000, 0.1300000000000020028 ) ) ;
#10724 = CARTESIAN_POINT ( 'NONE',  ( -0.2819296736111110424, 4.571611111186975940, -0.1167790944451423119 ) ) ;
#10725 = CARTESIAN_POINT ( 'NONE',  ( -0.2450779571127529310, 4.508096002043260775, 0.1931108503236894369 ) ) ;
#10726 = AXIS2_PLACEMENT_3D ( 'NONE', #5476, #24116, #1809 ) ;
#10727 = COORDINATED_UNIVERSAL_TIME_OFFSET ( 0, 0, .AHEAD. ) ;
#10728 = DIRECTION ( 'NONE',  ( 1.000000000000000000, 1.821231995776178240E-15, 0.000000000000000000 ) ) ;
#10729 = CARTESIAN_POINT ( 'NONE',  ( 0.1144950937579611444, 0.2764156081756483641, 0.2931944444444479769 ) ) ;
#10730 = CARTESIAN_POINT ( 'NONE',  ( 0.2819296736111110979, 4.061194444520309865, -3.452642723725051716E-17 ) ) ;
#10731 = CARTESIAN_POINT ( 'NONE',  ( -0.3098980794439091802, 4.834497018200990759, -0.03649681129806247454 ) ) ;
#10732 = CARTESIAN_POINT ( 'NONE',  ( 0.000000000000000000, 0.9099999999999988098, 0.000000000000000000 ) ) ;
#10733 = ADVANCED_FACE ( 'NONE', ( #17690 ), #19516, .T. ) ;
#10734 = CARTESIAN_POINT ( 'NONE',  ( 0.2764156081756483641, 0.1144950937579610195, 0.3487500000000039457 ) ) ;
#10735 = CC_DESIGN_APPROVAL ( #15656, ( #17744 ) ) ;
#10736 = CARTESIAN_POINT ( 'NONE',  ( 2.326421213736078119E-17, 0.1008928570453146989, -0.3799334167787516425 ) ) ;
#10737 = CARTESIAN_POINT ( 'NONE',  ( -0.2819296736111110979, 0.06319444436857780956, -3.452642723725051716E-17 ) ) ;
#10738 = CARTESIAN_POINT ( 'NONE',  ( 0.4687500000000002776, 0.04363579668119251659, 0.07944722321499816942 ) ) ;
#10739 = CARTESIAN_POINT ( 'NONE',  ( -0.02441201398332129568, 4.111524471938507119, -3.542879552481994043 ) ) ;
#10740 = DIRECTION ( 'NONE',  ( 1.493785812010397745E-17, -1.000000000000000000, 0.000000000000000000 ) ) ;
#10741 = CARTESIAN_POINT ( 'NONE',  ( 0.2764156081756483641, -0.1144950937579611028, 0.1126388888888909395 ) ) ;
#10742 = CARTESIAN_POINT ( 'NONE',  ( -0.2764156081756484196, -0.1144950937579609362, 0.04319444444444596465 ) ) ;
#10743 = ORIENTED_EDGE ( 'NONE', *, *, #18460, .T. ) ;
#10744 = VERTEX_POINT ( 'NONE', #862 ) ;
#10745 = CARTESIAN_POINT ( 'NONE',  ( 0.09135502326330754985, 0.5015332108058753180, 0.06108558933789665774 ) ) ;
#10746 = CARTESIAN_POINT ( 'NONE',  ( 0.1993543840281266910, 0.5979166665908001166, -0.1993543840281266910 ) ) ;
#10747 = CARTESIAN_POINT ( 'NONE',  ( -0.3119999999999999996, -0.009722222222222557178, -3.820898013339742174E-17 ) ) ;
#10748 = CARTESIAN_POINT ( 'NONE',  ( 0.1167790944451424368, 3.939666666742532186, 0.2819296736111110424 ) ) ;
#10749 = CARTESIAN_POINT ( 'NONE',  ( -0.3613381517857144343, -0.02053571438325666604, 0.1174058825155740171 ) ) ;
#10750 = AXIS2_PLACEMENT_3D ( 'NONE', #11670, #20923, #4334 ) ;
#10751 = CARTESIAN_POINT ( 'NONE',  ( 0.2819296736111110979, 4.394527777853643791, -3.452642723725051716E-17 ) ) ;
#10752 = PLANE ( 'NONE',  #20174 ) ;
#10753 = DIRECTION ( 'NONE',  ( -0.000000000000000000, -0.6546536707079746442, -0.7559289460184566156 ) ) ;
#10754 = ORIENTED_EDGE ( 'NONE', *, *, #16454, .F. ) ;
#10755 = CARTESIAN_POINT ( 'NONE',  ( -0.4687500000000003886, 0.2598076211353315124, 0.06112444011295379426 ) ) ;
#10756 = EDGE_CURVE ( 'NONE', #21992, #10917, #4640, .T. ) ;
#10757 = CARTESIAN_POINT ( 'NONE',  ( 5.731347020009612645E-17, 3.738277777929510215, 0.3119999999999999996 ) ) ;
#10758 = CC_DESIGN_APPROVAL ( #22227, ( #9980 ) ) ;
#10759 = CARTESIAN_POINT ( 'NONE',  ( 0.03516597121239248974, 4.209501246269358177, -0.3101320692603155571 ) ) ;
#10760 = B_SPLINE_CURVE_WITH_KNOTS ( 'NONE', 3,
 ( #12521, #22002, #13006, #14461, #18349, #10676, #5302, #18110, #1407, #12765, #3350, #18232, #1643, #1529, #8962, #7139, #9078, #12365, #16127, #4778, #21490, #23542, #10290, #23424, #5018, #17956, #8678, #8438, #23300, #6734, #12245, #15768, #885, #2957, #19659, #16005, #14177, #19782, #3082, #6612, #4903, #1130, #18071, #6857 ),
 .UNSPECIFIED., .F., .F.,
 ( 4, 2, 2, 2, 2, 2, 2, 2, 2, 2, 2, 2, 2, 2, 2, 2, 2, 2, 2, 2, 2, 4 ),
 ( 0.05299829238697165851, 0.05454307465341280692, 0.05608785691985395533, 0.05763263918629510374, 0.05840503031951568141, 0.05917742145273625909, 0.05994981258595682982, 0.06072220371917740750, 0.06226698598561855591, 0.06381176825205971126, 0.06535655051850086661, 0.06612894165172143734, 0.06690133278494202196, 0.06844611505138316343, 0.06999089731782431878, 0.07076328845104488952, 0.07153567958426546025, 0.07308046185070661560, 0.07462524411714777095, 0.07617002638358892630, 0.07694241751680949704, 0.07771480865003008165 ),
 .UNSPECIFIED. ) ;
#10761 = APPROVAL ( #12334, 'UNKNOWN' ) ;
#10762 = SHAPE_REPRESENTATION_RELATIONSHIP ( 'NONE' , 'NONE' ,  #11202, #4743 ) ;
#10763 = VECTOR ( 'NONE', #11479, 39.37007874015748143 ) ;
#10764 = CARTESIAN_POINT ( 'NONE',  ( 0.1167790944451422702, 5.002166666742532186, -0.2819296736111110979 ) ) ;
#10765 = APPROVAL_STATUS ( 'not_yet_approved' ) ;
#10766 = ORIENTED_EDGE ( 'NONE', *, *, #9928, .F. ) ;
#10767 = CIRCLE ( 'NONE', #20140, 0.01874999999999999584 ) ;
#10768 = CARTESIAN_POINT ( 'NONE',  ( -0.02336201496938555139, 4.070985353836114484, 0.3119999969656189198 ) ) ;
#10769 = LINE ( 'NONE', #20267, #2680 ) ;
#10770 = VERTEX_POINT ( 'NONE', #11985 ) ;
#10771 = CARTESIAN_POINT ( 'NONE',  ( 0.1167790944451423535, 0.2611111110352444808, 0.2819296736111110424 ) ) ;
#10772 = EDGE_LOOP ( 'NONE', ( #389, #1348, #1198 ) ) ;
#10773 = CARTESIAN_POINT ( 'NONE',  ( -0.2819296736111110979, 0.02499999992413337591, 0.1167790944451422425 ) ) ;
#10774 = LINE ( 'NONE', #18557, #7278 ) ;
#10775 = CARTESIAN_POINT ( 'NONE',  ( 1.573500000000000343, 0.5250000000000000222, -0.1650000000000001465 ) ) ;
#10776 = CARTESIAN_POINT ( 'NONE',  ( -0.1236067977499790416, -0.05000000000000000971, 0.3804226065180614236 ) ) ;
#10777 = CARTESIAN_POINT ( 'NONE',  ( -0.2206173157302027676, 4.502166666666665762, 0.2206173157302028787 ) ) ;
#10778 = CARTESIAN_POINT ( 'NONE',  ( -0.1292346314603983470, 3.783416666666665762, 0.3120000000000073270 ) ) ;
#10779 = LINE ( 'NONE', #14680, #1182 ) ;
#10780 = CC_DESIGN_SECURITY_CLASSIFICATION ( #15437, ( #24137 ) ) ;
#10781 = CYLINDRICAL_SURFACE ( 'NONE', #15873, 0.3119999999999999996 ) ;
#10782 = CARTESIAN_POINT ( 'NONE',  ( -0.2819296736111110979, 4.533416666742532186, 0.000000000000000000 ) ) ;
#10783 = DIRECTION ( 'NONE',  ( 0.7071067811865514585, -1.056266077312799537E-17, -0.7071067811865436870 ) ) ;
#10784 = CARTESIAN_POINT ( 'NONE',  ( -0.6288319206375506676, 3.738758431839877614E-19, 0.004799741732707325965 ) ) ;
#10785 = CARTESIAN_POINT ( 'NONE',  ( 0.1993543840281267465, 5.109805555631420582, 0.1993543840281266633 ) ) ;
#10786 = CARTESIAN_POINT ( 'NONE',  ( -0.09735099498061879075, 0.04500432081407945706, -0.2786451087458969300 ) ) ;
#10787 = FACE_OUTER_BOUND ( 'NONE', #10772, .T. ) ;
#10788 = PLANE ( 'NONE',  #4322 ) ;
#10789 = DIRECTION ( 'NONE',  ( 0.000000000000000000, 0.000000000000000000, 1.000000000000000000 ) ) ;
#10790 = CARTESIAN_POINT ( 'NONE',  ( -0.1292346314604057023, 4.290361111262844140, 0.3119999999999998885 ) ) ;
#10791 = CARTESIAN_POINT ( 'NONE',  ( -0.2819296736111110979, 4.529944444520310753, -0.1167790944451422980 ) ) ;
#10792 = CARTESIAN_POINT ( 'NONE',  ( -1.726321361862525858E-17, 3.894527777853643347, -0.2819296736111110979 ) ) ;
#10793 = VERTEX_POINT ( 'NONE', #19398 ) ;
#10794 = EDGE_CURVE ( 'NONE', #10448, #4062, #21581, .T. ) ;
#10795 = ORIENTED_EDGE ( 'NONE', *, *, #19305, .T. ) ;
#10796 = ORIENTED_EDGE ( 'NONE', *, *, #12915, .F. ) ;
#10797 = DATE_AND_TIME ( #12757, #4871 ) ;
#10798 = CARTESIAN_POINT ( 'NONE',  ( -0.08700723303875142201, -0.2927098606306429707, 0.4165748844700365994 ) ) ;
#10799 = LINE ( 'NONE', #18227, #12270 ) ;
#10800 = EDGE_LOOP ( 'NONE', ( #8953, #10193, #19808, #17288 ) ) ;
#10801 = CARTESIAN_POINT ( 'NONE',  ( 0.3119999999999999996, 0.3479166665149338034, -0.1292346314604056468 ) ) ;
#10802 = VECTOR ( 'NONE', #21937, 39.37007874015748854 ) ;
#10803 = CARTESIAN_POINT ( 'NONE',  ( -0.2214530096782409696, 4.384127800144598908, -0.2198004540226814463 ) ) ;
#10804 = DIRECTION ( 'NONE',  ( 0.000000000000000000, 0.000000000000000000, 1.000000000000000000 ) ) ;
#10805 = CYLINDRICAL_SURFACE ( 'NONE', #7230, 0.2500000000000000000 ) ;
#10806 = CARTESIAN_POINT ( 'NONE',  ( 0.1067006177585113069, 0.5609178672485701789, -0.7424598444660861496 ) ) ;
#10807 = ORIENTED_EDGE ( 'NONE', *, *, #14190, .F. ) ;
#10808 = CARTESIAN_POINT ( 'NONE',  ( 0.2253486499796795439, 5.092611837936364516, -0.2157528262157012711 ) ) ;
#10809 = CARTESIAN_POINT ( 'NONE',  ( -0.1144950937579609918, -0.2764156081756484196, 0.3209722222222259891 ) ) ;
#10810 = CARTESIAN_POINT ( 'NONE',  ( -0.2819296736111110979, 4.186194444520309865, 0.000000000000000000 ) ) ;
#10811 = CARTESIAN_POINT ( 'NONE',  ( -0.1993543840281266910, 5.179250000075866112, -0.1993543840281266910 ) ) ;
#10812 = EDGE_CURVE ( 'NONE', #280, #1241, #9105, .T. ) ;
#10813 = DIRECTION ( 'NONE',  ( -0.000000000000000000, -1.000000000000000000, -0.000000000000000000 ) ) ;
#10814 = CARTESIAN_POINT ( 'NONE',  ( -0.03304210309726871020, 4.237377706265436750, 0.3102558678455366592 ) ) ;
#10815 = CARTESIAN_POINT ( 'NONE',  ( -0.2206173157302027676, 4.113277777777777366, 0.2206173157302028787 ) ) ;
#10816 = EDGE_CURVE ( 'NONE', #1066, #2961, #1103, .T. ) ;
#10817 = CARTESIAN_POINT ( 'NONE',  ( 0.1292346314604058410, 4.963972222373953969, 0.3119999999999998885 ) ) ;
#10818 = CARTESIAN_POINT ( 'NONE',  ( -0.2819296736111110979, 5.144527777853643791, 0.000000000000000000 ) ) ;
#10819 = VECTOR ( 'NONE', #19721, 39.37007874015748854 ) ;
#10820 = CARTESIAN_POINT ( 'NONE',  ( -0.2209708691207961095, 0.2209708691207961373, 0.2202777777777805146 ) ) ;
#10821 = ORIENTED_EDGE ( 'NONE', *, *, #3946, .F. ) ;
#10822 = EDGE_CURVE ( 'NONE', #20713, #7372, #19866, .T. ) ;
#10823 = CARTESIAN_POINT ( 'NONE',  ( -0.0006132284040734684288, 4.877183144895580469, -0.3119999996348461480 ) ) ;
#10824 = CARTESIAN_POINT ( 'NONE',  ( 0.2230971623002954429, 0.2230971623002953319, 0.3227083333333373161 ) ) ;
#10825 = CARTESIAN_POINT ( 'NONE',  ( 0.2233192592356399997, 0.3794642856167432798, -0.3073725909049500049 ) ) ;
#10826 = ORIENTED_EDGE ( 'NONE', *, *, #12675, .F. ) ;
#10827 = CARTESIAN_POINT ( 'NONE',  ( 0.1953806383669984825, -0.4284628132096562347, 0.4289620446068268533 ) ) ;
#10828 = DIRECTION ( 'NONE',  ( 0.8660254037844361541, 0.000000000000000000, 0.5000000000000042188 ) ) ;
#10829 = CIRCLE ( 'NONE', #13948, 0.03000000000000002318 ) ;
#10830 = CARTESIAN_POINT ( 'NONE',  ( -0.1993543840281267465, 0.1951388888130222710, 0.1993543840281266633 ) ) ;
#10831 = CARTESIAN_POINT ( 'NONE',  ( -0.1144950937579609918, -0.2764156081756484196, 0.1612500000000023914 ) ) ;
#10832 = CARTESIAN_POINT ( 'NONE',  ( 0.000000000000000000, 0.01999999999999951469, 1.243000000000000105 ) ) ;
#10833 = CARTESIAN_POINT ( 'NONE',  ( 0.3133630161831524874, 4.474762566377171957, -0.01146161691659670044 ) ) ;
#10834 = VERTEX_POINT ( 'NONE', #2809 ) ;
#10835 = CARTESIAN_POINT ( 'NONE',  ( -0.1005150341732207325, 3.768858437468117994, -0.2960704298912133492 ) ) ;
#10836 = CARTESIAN_POINT ( 'NONE',  ( -0.1940126398823881770, 4.605354529194622515, -0.2443523765828770344 ) ) ;
#10837 = LINE ( 'NONE', #23982, #18323 ) ;
#10838 = CARTESIAN_POINT ( 'NONE',  ( 5.731347020009612645E-17, 4.842444444444443441, 0.3119999999999999996 ) ) ;
#10839 = DIRECTION ( 'NONE',  ( 0.000000000000000000, 0.000000000000000000, -1.000000000000000000 ) ) ;
#10840 = CARTESIAN_POINT ( 'NONE',  ( -0.3119999999999999996, 4.772999999999998799, 0.000000000000000000 ) ) ;
#10841 = CARTESIAN_POINT ( 'NONE',  ( -0.1167790944451423535, 4.085500000075865223, 0.2819296736111110979 ) ) ;
#10842 = CARTESIAN_POINT ( 'NONE',  ( 0.1993543840281267465, 3.776472222298087988, 0.1993543840281266633 ) ) ;
#10843 = CARTESIAN_POINT ( 'NONE',  ( 0.2959623242263846321, 4.032775975072071972, -0.09874543881575856275 ) ) ;
#10844 = EDGE_LOOP ( 'NONE', ( #11759, #10075, #14822, #23971, #16882, #17462, #13819, #18224, #12709, #3577, #20147, #3788, #4683, #20919, #7719, #16690, #8831, #23498, #6516, #7423, #10443, #23459, #2128, #7751, #9448 ) ) ;
#10845 = FACE_OUTER_BOUND ( 'NONE', #18135, .T. ) ;
#10846 = ORIENTED_EDGE ( 'NONE', *, *, #2081, .T. ) ;
#10847 = CARTESIAN_POINT ( 'NONE',  ( 0.2819296736111110979, 4.543833333409199149, 0.1167790944451422425 ) ) ;
#10848 = ADVANCED_FACE ( 'NONE', ( #10264 ), #6708, .T. ) ;
#10849 = CARTESIAN_POINT ( 'NONE',  ( -0.2019846619707756641, 4.509905506849337442, 0.2387847868100533566 ) ) ;
#10850 = CIRCLE ( 'NONE', #20950, 0.4624999999999992450 ) ;
#10851 = LINE ( 'NONE', #23867, #8033 ) ;
#10852 = CARTESIAN_POINT ( 'NONE',  ( 0.1144950937579609085, -0.2764156081756484751, 0.1612500000000025024 ) ) ;
#10853 = CARTESIAN_POINT ( 'NONE',  ( 0.1167790944451424506, 3.828555555631421470, 0.2819296736111110424 ) ) ;
#10854 = CARTESIAN_POINT ( 'NONE',  ( 0.000000000000000000, 5.580000000000000959, 0.2500000000000000555 ) ) ;
#10855 = CARTESIAN_POINT ( 'NONE',  ( 0.1522808163552602789, 5.156853442606030846, -0.2598339165385931127 ) ) ;
#10856 = CARTESIAN_POINT ( 'NONE',  ( 0.000000000000000000, 6.000000000000000888, 0.000000000000000000 ) ) ;
#10857 = CARTESIAN_POINT ( 'NONE',  ( 0.2923287055106771337, 0.07589285704531473220, 0.2123892367102621359 ) ) ;
#10858 = CARTESIAN_POINT ( 'NONE',  ( -0.1993543840281267465, 0.2368055554796889561, 0.1993543840281266633 ) ) ;
#10859 = DIRECTION ( 'NONE',  ( -0.000000000000000000, 0.000000000000000000, 1.000000000000000000 ) ) ;
#10860 = CARTESIAN_POINT ( 'NONE',  ( 0.3236067977499789694, 0.02678571409062948175, 0.2351141009169893659 ) ) ;
#10861 = CARTESIAN_POINT ( 'NONE',  ( -0.09471748901421209177, 0.5680892572981176558, -0.7441037951239753978 ) ) ;
#10862 = CARTESIAN_POINT ( 'NONE',  ( -0.1144950937579609779, 0.2764156081756484196, -0.03319444444444354797 ) ) ;
#10863 = CARTESIAN_POINT ( 'NONE',  ( 0.2764156081756483641, 0.1144950937579610056, 0.07097222222222394905 ) ) ;
#10864 = VERTEX_POINT ( 'NONE', #14038 ) ;
#10865 = VERTEX_POINT ( 'NONE', #10028 ) ;
#10866 = CARTESIAN_POINT ( 'NONE',  ( 3.061616997868383634E-17, 0.4199999999999998734, 0.2500000000000000555 ) ) ;
#10867 = CARTESIAN_POINT ( 'NONE',  ( 5.731347020009612645E-17, 4.731333333333332725, 0.3119999999999999996 ) ) ;
#10868 = CARTESIAN_POINT ( 'NONE',  ( 0.1292346314604057023, 0.1187499999999996614, 0.3119999999999998885 ) ) ;
#10869 = CARTESIAN_POINT ( 'NONE',  ( 0.2819296736111110979, 3.891055555631421914, 0.1167790944451422425 ) ) ;
#10870 = CARTESIAN_POINT ( 'NONE',  ( 0.3613381517857143232, 0.1544642856167432743, 0.000000000000000000 ) ) ;
#10871 = CARTESIAN_POINT ( 'NONE',  ( -0.2819296736111110424, 4.474388888964755395, -0.1167790944451423119 ) ) ;
#10872 = CARTESIAN_POINT ( 'NONE',  ( 0.1292346314604057300, 0.1118055554038226290, 0.3119999999999998885 ) ) ;
#10873 = CARTESIAN_POINT ( 'NONE',  ( 0.3003475124358454540, 1.999640111863030256, -3.545613612297686679 ) ) ;
#10874 = ORIENTED_EDGE ( 'NONE', *, *, #9482, .T. ) ;
#10875 = CARTESIAN_POINT ( 'NONE',  ( 0.06335377612981443751, 0.3839733671981016006, 0.4000000000000000222 ) ) ;
#10876 = EDGE_CURVE ( 'NONE', #6859, #3037, #15542, .T. ) ;
#10877 = CARTESIAN_POINT ( 'NONE',  ( 0.1993543840281266633, 5.109805555631420582, -0.1993543840281266910 ) ) ;
#10878 = EDGE_CURVE ( 'NONE', #14303, #19328, #16345, .T. ) ;
#10879 = CARTESIAN_POINT ( 'NONE',  ( 0.2387648180985315616, 4.202823093931177922, -0.2008770064554694090 ) ) ;
#10880 = DIRECTION ( 'NONE',  ( -0.000000000000000000, 0.2588190451025213501, -0.9659258262890682012 ) ) ;
#10881 = CARTESIAN_POINT ( 'NONE',  ( 0.000000000000000000, 0.4997679491924311157, 0.000000000000000000 ) ) ;
#10882 = AXIS2_PLACEMENT_3D ( 'NONE', #21411, #17754, #6994 ) ;
#10883 = CARTESIAN_POINT ( 'NONE',  ( -0.2819296736111110424, 4.634111111186976828, 0.1167790944451424923 ) ) ;
#10884 = APPROVAL_DATE_TIME ( #1488, #8209 ) ;
#10885 = CARTESIAN_POINT ( 'NONE',  ( -0.2104324251216644903, 4.065027146098090682, 0.2311922143307865718 ) ) ;
#10886 = DIRECTION ( 'NONE',  ( 0.000000000000000000, 0.000000000000000000, 1.000000000000000000 ) ) ;
#10887 = CARTESIAN_POINT ( 'NONE',  ( -0.1167790944451422702, 0.2333333332574666907, -0.2819296736111110424 ) ) ;
#10888 = ORIENTED_EDGE ( 'NONE', *, *, #20063, .T. ) ;
#10889 = CARTESIAN_POINT ( 'NONE',  ( -0.1167790944451424368, 0.1430555554796889284, 0.2819296736111110424 ) ) ;
#10890 = DIRECTION ( 'NONE',  ( 0.000000000000000000, 0.000000000000000000, -1.000000000000000000 ) ) ;
#10891 = CARTESIAN_POINT ( 'NONE',  ( -0.1324640314579201839, 5.193749668861634028, -0.2568599863705673947 ) ) ;
#10892 = CARTESIAN_POINT ( 'NONE',  ( -0.3236067977499790249, -0.05714285714285716189, 0.2351141009169892271 ) ) ;
#10893 = CARTESIAN_POINT ( 'NONE',  ( -0.3155070326520292845, 1.931923388228935888E-17, -0.1043749999999998707 ) ) ;
#10894 = CARTESIAN_POINT ( 'NONE',  ( 0.3125000000000000000, -5.740531871003217465E-17, 0.4216666666666709085 ) ) ;
#10895 = CARTESIAN_POINT ( 'NONE',  ( 0.1797084794423411680, 3.735609856212664948, -0.2172307604343298448 ) ) ;
#10896 = CARTESIAN_POINT ( 'NONE',  ( 0.1167790944451423257, 0.1013888888130222432, -0.2819296736111110424 ) ) ;
#10897 = CARTESIAN_POINT ( 'NONE',  ( -0.1993543840281266355, 4.540361111186976828, 0.1993543840281267465 ) ) ;
#10898 = CARTESIAN_POINT ( 'NONE',  ( 2.575339694675500462E-17, 0.05178571409062950742, -0.4205848896953069405 ) ) ;
#10899 = FACE_OUTER_BOUND ( 'NONE', #546, .T. ) ;
#10900 = CARTESIAN_POINT ( 'NONE',  ( 0.2819296736111110979, 5.061194444520310753, -3.452642723725051716E-17 ) ) ;
#10901 = PRODUCT_DEFINITION ( 'UNKNOWN', '', #582, #15817 ) ;
#10902 = CARTESIAN_POINT ( 'NONE',  ( -0.2621650492421670475, 0.04909780403330635951, -0.1442773403164986090 ) ) ;
#10903 = CARTESIAN_POINT ( 'NONE',  ( 0.1113886448093519416, 3.762860911357303273, -0.2917950463651685089 ) ) ;
#10904 = CARTESIAN_POINT ( 'NONE',  ( -0.2206173157302027954, 0.4763888887371559577, -0.2206173157302028232 ) ) ;
#10905 = CIRCLE ( 'NONE', #17892, 0.3119999999999999996 ) ;
#10906 = FACE_OUTER_BOUND ( 'NONE', #22657, .T. ) ;
#10907 = CARTESIAN_POINT ( 'NONE',  ( 0.1292346314604056190, 4.262583333485065573, -0.3119999999999999996 ) ) ;
#10908 = CARTESIAN_POINT ( 'NONE',  ( -0.1167790944451423535, 4.543833333409198261, 0.2819296736111110979 ) ) ;
#10909 = CARTESIAN_POINT ( 'NONE',  ( 5.178964085587577574E-17, 3.755638888964754951, 0.2819296736111110979 ) ) ;
#10910 = EDGE_LOOP ( 'NONE', ( #21994, #1129, #11264, #5721 ) ) ;
#10911 = PRODUCT ( 'Aloris-BXA-Top-Bushing', 'Aloris-BXA-Top-Bushing', '', ( #7957 ) ) ;
#10912 = EDGE_LOOP ( 'NONE', ( #18435, #1910, #19064, #6184 ) ) ;
#10913 = ORIENTED_EDGE ( 'NONE', *, *, #20792, .T. ) ;
#10914 = APPROVAL_ROLE ( '' ) ;
#10915 = LINE ( 'NONE', #19935, #22397 ) ;
#10916 = CARTESIAN_POINT ( 'NONE',  ( -0.5116234456863258950, 4.559812086079793048, -2.813986238491759551 ) ) ;
#10917 = VERTEX_POINT ( 'NONE', #3054 ) ;
#10918 = CARTESIAN_POINT ( 'NONE',  ( -0.1292346314604058410, 0.2715277776260447973, 0.3119999999999998885 ) ) ;
#10919 = CARTESIAN_POINT ( 'NONE',  ( -0.2801425706040142072, 4.395165469185563722, 0.1388625805350480191 ) ) ;
#10920 = EDGE_CURVE ( 'NONE', #2537, #6278, #12940, .T. ) ;
#10921 = FACE_OUTER_BOUND ( 'NONE', #12397, .T. ) ;
#10922 = CARTESIAN_POINT ( 'NONE',  ( 5.731347020009612645E-17, 4.953555555555554157, 0.3119999999999999996 ) ) ;
#10923 = CARTESIAN_POINT ( 'NONE',  ( -8.183246661411124563E-08, 3.960496777434589610, 0.3119999999999772400 ) ) ;
#10924 = EDGE_LOOP ( 'NONE', ( #8458, #18757 ) ) ;
#10925 = CARTESIAN_POINT ( 'NONE',  ( 0.3613381517857143232, 0.2258928570453146989, 0.000000000000000000 ) ) ;
#10926 =( REPRESENTATION_RELATIONSHIP ('NONE','NONE', #4490, #20236 ) REPRESENTATION_RELATIONSHIP_WITH_TRANSFORMATION ( #21731 )SHAPE_REPRESENTATION_RELATIONSHIP( ) );
#10927 = CARTESIAN_POINT ( 'NONE',  ( 0.1913867056871989270, 5.077500454502875904, 0.2465551918856197511 ) ) ;
#10928 = CARTESIAN_POINT ( 'NONE',  ( 0.2764156081756483641, -0.1144950937579611167, 0.2793055555555589153 ) ) ;
#10929 = ADVANCED_FACE ( 'NONE', ( #22064 ), #5066, .T. ) ;
#10930 = CARTESIAN_POINT ( 'NONE',  ( 0.1993543840281267465, 4.262583333409199149, 0.1993543840281266633 ) ) ;
#10931 = CARTESIAN_POINT ( 'NONE',  ( -1.726321361862525858E-17, 5.061194444520309865, -0.2819296736111110979 ) ) ;
#10932 = CARTESIAN_POINT ( 'NONE',  ( 0.2744310710835856093, -0.1177455570400168794, 0.4097706279014594610 ) ) ;
#10933 = CARTESIAN_POINT ( 'NONE',  ( -0.2052485393096138977, 4.231925960476026205, 0.2359794098173954580 ) ) ;
#10934 = CARTESIAN_POINT ( 'NONE',  ( 0.3119999999999999996, 3.970916666666665762, -0.1292346314604056745 ) ) ;
#10935 = CARTESIAN_POINT ( 'NONE',  ( -0.1292346314604056745, 4.936194444596176290, -0.3119999999999999996 ) ) ;
#10936 = CARTESIAN_POINT ( 'NONE',  ( 0.2819296736111110979, 5.064666666742532186, -0.1167790944451423396 ) ) ;
#10937 = CIRCLE ( 'NONE', #6638, 0.6288319206375507786 ) ;
#10938 = CARTESIAN_POINT ( 'NONE',  ( -0.3119999999999999996, 4.161888888888888083, 0.000000000000000000 ) ) ;
#10939 = VERTEX_POINT ( 'NONE', #12824 ) ;
#10940 = CARTESIAN_POINT ( 'NONE',  ( 1.573500000000000343, 0.5250000000000000222, -0.3524999999999999800 ) ) ;
#10941 = CARTESIAN_POINT ( 'NONE',  ( 0.02274447101932148066, 0.04271007974323598466, -0.2915486118860042275 ) ) ;
#10942 = ORIENTED_EDGE ( 'NONE', *, *, #22479, .T. ) ;
#10943 = CARTESIAN_POINT ( 'NONE',  ( 0.2230971623002953874, -0.2230971623002954429, 0.3643750000000042788 ) ) ;
#10944 = CARTESIAN_POINT ( 'NONE',  ( 0.2819296736111110424, 5.217444444520309865, -0.1167790944451423396 ) ) ;
#10945 = VERTEX_POINT ( 'NONE', #20243 ) ;
#10946 = CARTESIAN_POINT ( 'NONE',  ( 0.3838430204063560391, -0.3081239094298764414, 0.4164750180373182897 ) ) ;
#10947 = CARTESIAN_POINT ( 'NONE',  ( 1.573500000000000343, 0.000000000000000000, -1.006250000000000311 ) ) ;
#10948 = AXIS2_PLACEMENT_3D ( 'NONE', #1209, #23258, #21087 ) ;
#10949 = CARTESIAN_POINT ( 'NONE',  ( 0.2819296736111110979, 0.2715277777019111660, 0.000000000000000000 ) ) ;
#10950 = CARTESIAN_POINT ( 'NONE',  ( -0.2764156081756484196, 0.1144950937579609918, 0.2029166666666694097 ) ) ;
#10951 = CARTESIAN_POINT ( 'NONE',  ( 0.2819296736111110979, 5.224388888964754507, 0.1167790944451422425 ) ) ;
#10952 = LINE ( 'NONE', #14486, #9310 ) ;
#10953 = ADVANCED_FACE ( 'NONE', ( #1702 ), #24006, .T. ) ;
#10954 = EDGE_LOOP ( 'NONE', ( #17693, #7838, #21613 ) ) ;
#10955 = B_SPLINE_CURVE_WITH_KNOTS ( 'NONE', 3,
 ( #17052, #5830, #708, #2542, #7897, #13296, #6312, #4006, #20951, #346, #11819, #7785, #4246, #587, #15232, #11696, #21070, #4361 ),
 .UNSPECIFIED., .F., .F.,
 ( 4, 2, 2, 2, 2, 2, 2, 2, 4 ),
 ( 0.5939386199298102298, 0.5962229759072257274, 0.5985073318846413359, 0.6007916878620569445, 0.6030760438394724421, 0.6053603998168879397, 0.6076447557943035482, 0.6099291117717191568, 0.6122134677491346544 ),
 .UNSPECIFIED. ) ;
#10956 = CARTESIAN_POINT ( 'NONE',  ( 5.178964085587577574E-17, 4.977861111186976828, 0.2819296736111110979 ) ) ;
#10957 = CARTESIAN_POINT ( 'NONE',  ( -0.3119612969836771388, 4.167620540232060300, -0.04114099006773573597 ) ) ;
#10958 = CARTESIAN_POINT ( 'NONE',  ( -0.3119999999999999996, 5.047305555555555046, -0.1292346314604056468 ) ) ;
#10959 = CARTESIAN_POINT ( 'NONE',  ( 0.3119999999999999996, 4.582027777777776478, -0.1292346314604056745 ) ) ;
#10960 = CARTESIAN_POINT ( 'NONE',  ( 0.3950000000000000178, 0.04999999999999921868, 1.768075471041792386E-33 ) ) ;
#10961 = CARTESIAN_POINT ( 'NONE',  ( -1.910449006669871087E-17, 4.647999999999998799, -0.3119999999999999996 ) ) ;
#10962 = CARTESIAN_POINT ( 'NONE',  ( 0.1993543840281266633, 3.998694444520309865, -0.1993543840281266910 ) ) ;
#10963 = CARTESIAN_POINT ( 'NONE',  ( 0.1015009281151166981, 3.738732047420452620, -0.2819296736111110979 ) ) ;
#10964 = CARTESIAN_POINT ( 'NONE',  ( 0.02511968257364222828, 4.043153853174205281, -0.3113283232506174336 ) ) ;
#10965 = CARTESIAN_POINT ( 'NONE',  ( 0.003278813451167444763, 0.5383665848074060678, 0.05892894635879485088 ) ) ;
#10966 = B_SPLINE_CURVE_WITH_KNOTS ( 'NONE', 3,
 ( #21538, #6664, #17888, #4598, #10338, #6305, #10219, #2536, #17643, #9982 ),
 .UNSPECIFIED., .F., .F.,
 ( 4, 2, 2, 2, 4 ),
 ( 0.000000000000000000, 0.003321633220911225995, 0.006643266441822451990, 0.009964899662733677985, 0.01328653288364490398 ),
 .UNSPECIFIED. ) ;
#10967 = ORIENTED_EDGE ( 'NONE', *, *, #10975, .T. ) ;
#10968 = DIRECTION ( 'NONE',  ( -0.000000000000000000, -1.000000000000000000, -0.000000000000000000 ) ) ;
#10969 = ORIENTED_EDGE ( 'NONE', *, *, #23301, .T. ) ;
#10970 = CARTESIAN_POINT ( 'NONE',  ( 0.1167790944451422702, 4.391055555631420582, -0.2819296736111110424 ) ) ;
#10971 = CARTESIAN_POINT ( 'NONE',  ( -0.3037587743577567778, 4.111198837271344608, -0.07370139431766779825 ) ) ;
#10972 = DIRECTION ( 'NONE',  ( 0.000000000000000000, 1.000000000000000000, 0.000000000000000000 ) ) ;
#10973 = CARTESIAN_POINT ( 'NONE',  ( -0.1954553509668046918, -0.1954553509668046640, 0.1508333333333357063 ) ) ;
#10974 = ADVANCED_FACE ( 'NONE', ( #6832, #21709 ), #8774, .T. ) ;
#10975 = EDGE_CURVE ( 'NONE', #4825, #6378, #15003, .T. ) ;
#10976 = CARTESIAN_POINT ( 'NONE',  ( -0.3120000142875944960, 3.947771082080143934, 0.04084060482829639932 ) ) ;
#10977 = FACE_OUTER_BOUND ( 'NONE', #4369, .T. ) ;
#10978 = CARTESIAN_POINT ( 'NONE',  ( -0.1954553509668046640, 0.1954553509668046918, 0.3661111111111151617 ) ) ;
#10979 = CARTESIAN_POINT ( 'NONE',  ( -0.2233192592356399442, 0.2508928570453147211, -0.3073725909049500049 ) ) ;
#10980 = CARTESIAN_POINT ( 'NONE',  ( -0.2819296736111110979, 0.2298611110352444808, -3.452642723725051716E-17 ) ) ;
#10981 = CARTESIAN_POINT ( 'NONE',  ( 0.000000000000000000, 5.501232050807569607, -0.2499999999999999722 ) ) ;
#10982 = DIRECTION ( 'NONE',  ( -0.000000000000000000, 1.000000000000000000, -0.000000000000000000 ) ) ;
#10983 = CARTESIAN_POINT ( 'NONE',  ( -0.07574842331155759445, 0.5769426278466130986, -0.7461920942536031109 ) ) ;
#10984 = CARTESIAN_POINT ( 'NONE',  ( 0.2764156081756483641, 0.1144950937579610056, 0.01541666666666794208 ) ) ;
#10985 = EDGE_CURVE ( 'NONE', #10393, #23965, #13285, .T. ) ;
#10986 = ORIENTED_EDGE ( 'NONE', *, *, #6488, .F. ) ;
#10987 = ORIENTED_EDGE ( 'NONE', *, *, #11833, .T. ) ;
#10988 = LINE ( 'NONE', #20483, #10677 ) ;
#10989 = CARTESIAN_POINT ( 'NONE',  ( 5.731347020009612645E-17, 4.342444444444443441, 0.3119999999999999996 ) ) ;
#10990 = CARTESIAN_POINT ( 'NONE',  ( 0.1292346314604056745, -0.02708333333333366733, -0.3119999999999999996 ) ) ;
#10991 = CARTESIAN_POINT ( 'NONE',  ( -0.2819296736111110424, 3.752166666742533074, -0.1167790944451423119 ) ) ;
#10992 = CARTESIAN_POINT ( 'NONE',  ( -0.2233192592356399997, 0.1294642856167433076, 0.3073725909049499494 ) ) ;
#10993 = CARTESIAN_POINT ( 'NONE',  ( -0.1993543840281266355, 4.373694444520309865, 0.1993543840281267465 ) ) ;
#10994 = CARTESIAN_POINT ( 'NONE',  ( 0.5997114317030027841, 2.978485840173427324, -1.206013144887902788 ) ) ;
#10995 = ORIENTED_EDGE ( 'NONE', *, *, #20666, .T. ) ;
#10996 = CARTESIAN_POINT ( 'NONE',  ( 0.2634491424827775097, 4.358245445987300570, 0.1671768415365145755 ) ) ;
#10997 = CARTESIAN_POINT ( 'NONE',  ( 0.1167790944451424368, 4.870222222298087544, 0.2819296736111110424 ) ) ;
#10998 = EDGE_CURVE ( 'NONE', #17107, #18221, #9749, .T. ) ;
#10999 = CARTESIAN_POINT ( 'NONE',  ( 0.2933062516910102668, 4.193495950309771736, 0.1074496315832312171 ) ) ;
#11000 = DIRECTION ( 'NONE',  ( -1.000000000000000000, 0.000000000000000000, 0.000000000000000000 ) ) ;
#11001 = CARTESIAN_POINT ( 'NONE',  ( 0.1993543840281266633, 4.609805555631420582, -0.1993543840281266910 ) ) ;
#11002 = COORDINATED_UNIVERSAL_TIME_OFFSET ( 0, 0, .AHEAD. ) ;
#11003 = CARTESIAN_POINT ( 'NONE',  ( -0.4683396222371151718, 0.2655382811872564197, 0.04698599556840152291 ) ) ;
#11004 = FACE_OUTER_BOUND ( 'NONE', #16314, .T. ) ;
#11005 = DIRECTION ( 'NONE',  ( -0.000000000000000000, 1.000000000000000000, -0.000000000000000000 ) ) ;
#11006 = ORIENTED_EDGE ( 'NONE', *, *, #16283, .F. ) ;
#11007 = CARTESIAN_POINT ( 'NONE',  ( -0.1167790944451422702, 0.2888888888130222710, -0.2819296736111110424 ) ) ;
#11008 = EDGE_CURVE ( 'NONE', #20991, #8464, #5598, .T. ) ;
#11009 = CARTESIAN_POINT ( 'NONE',  ( -0.05541411813196098213, 4.712050423989051495, -0.3078451288426665711 ) ) ;
#11010 = DIRECTION ( 'NONE',  ( 0.4999999999999916178, 0.000000000000000000, -0.8660254037844433705 ) ) ;
#11011 = CARTESIAN_POINT ( 'NONE',  ( 0.4000000000000000222, -0.02857142857142858788, 0.000000000000000000 ) ) ;
#11012 = DIRECTION ( 'NONE',  ( -0.000000000000000000, -1.000000000000000000, -0.000000000000000000 ) ) ;
#11013 = CONICAL_SURFACE ( 'NONE', #7508, 0.2124999999999999944, 0.7853981633974463916 ) ;
#11014 = EDGE_CURVE ( 'NONE', #10162, #12271, #17186, .T. ) ;
#11015 =( BOUNDED_CURVE ( )  B_SPLINE_CURVE ( 2, ( #2534, #457, #5942, #7777, #17406, #11324, #7889, #19227, #9979 ),
 .UNSPECIFIED., .F., .F. ) 
 B_SPLINE_CURVE_WITH_KNOTS ( ( 3, 2, 2, 2, 3 ),
 ( 0.8125000000000002220, 0.8169642857142858094, 0.8214285714285713969, 0.8258928571428569843, 0.8303571428571426827 ),
 .UNSPECIFIED. ) 
 CURVE ( )  GEOMETRIC_REPRESENTATION_ITEM ( )  RATIONAL_B_SPLINE_CURVE ( ( 0.9999999999999962252, 0.9238795325112905132, 1.000000000000000000, 0.9238795325112867385, 1.000000000000000000, 0.9238795325112867385, 1.000000000000000000, 0.9238795325112905132, 0.9999999999999962252 ) ) 
 REPRESENTATION_ITEM ( '' )  );
#11016 = CARTESIAN_POINT ( 'NONE',  ( -0.3119999999999999996, 3.769527777777777811, -0.1292346314604056468 ) ) ;
#11017 = PLANE ( 'NONE',  #6623 ) ;
#11018 = CARTESIAN_POINT ( 'NONE',  ( 0.1167790944451423535, 0.02499999992413337591, 0.2819296736111110424 ) ) ;
#11019 = CARTESIAN_POINT ( 'NONE',  ( -0.2819296736111110424, 4.592444444520309865, 0.1167790944451424923 ) ) ;
#11020 = CARTESIAN_POINT ( 'NONE',  ( 0.3999999999999999667, 0.1803571426620581009, -0.1299678784931625475 ) ) ;
#11021 = DIRECTION ( 'NONE',  ( 0.000000000000000000, 0.7071067811865416886, 0.7071067811865531239 ) ) ;
#11022 = CARTESIAN_POINT ( 'NONE',  ( -0.2819296736111110424, 5.196611111186976828, -0.1167790944451423119 ) ) ;
#11023 = CARTESIAN_POINT ( 'NONE',  ( 0.1993543840281267465, 4.373694444520309865, 0.1993543840281266633 ) ) ;
#11024 = CARTESIAN_POINT ( 'NONE',  ( 0.02043441368966909463, 4.932131780984220448, -0.3120000003117849863 ) ) ;
#11025 = CARTESIAN_POINT ( 'NONE',  ( 0.000000000000000000, -3.937007874019685528E-05, 0.7500000000000001110 ) ) ;
#11026 = CARTESIAN_POINT ( 'NONE',  ( -0.3096487991955141350, 0.3624900597954727188, 0.07655254331177274718 ) ) ;
#11027 = CARTESIAN_POINT ( 'NONE',  ( 0.1292346314604058410, 4.352861111262843252, 0.3119999999999998885 ) ) ;
#11028 = CARTESIAN_POINT ( 'NONE',  ( 0.2819296736111110979, 4.564666666742532186, -0.1167790944451423396 ) ) ;
#11029 = CARTESIAN_POINT ( 'NONE',  ( 0.2819296736111110979, 3.766055555631420582, 0.1167790944451422425 ) ) ;
#11030 = VECTOR ( 'NONE', #22494, 39.37007874015748854 ) ;
#11031 = ORIENTED_EDGE ( 'NONE', *, *, #23749, .T. ) ;
#11032 = ORIENTED_EDGE ( 'NONE', *, *, #16756, .T. ) ;
#11033 = APPROVAL_DATE_TIME ( #19934, #13438 ) ;
#11034 = CARTESIAN_POINT ( 'NONE',  ( 0.2206173157302028787, 4.238277777777777366, 0.2206173157302027954 ) ) ;
#11035 = DIRECTION ( 'NONE',  ( -0.000000000000000000, 1.000000000000000000, -0.000000000000000000 ) ) ;
#11036 = EDGE_LOOP ( 'NONE', ( #23307, #6769, #6370, #3347 ) ) ;
#11037 = CARTESIAN_POINT ( 'NONE',  ( -0.1292346314604056190, 0.4729166665149337478, -0.3119999999999999996 ) ) ;
#11038 = LINE ( 'NONE', #5419, #19845 ) ;
#11039 = CARTESIAN_POINT ( 'NONE',  ( -0.1072922602170164191, 3.735183360884210657, 0.2929731678372050618 ) ) ;
#11040 = CARTESIAN_POINT ( 'NONE',  ( -0.009375000000000190473, 0.5358532185916217161, 0.3779506566538943790 ) ) ;
#11041 = DIRECTION ( 'NONE',  ( -0.000000000000000000, -0.000000000000000000, -1.000000000000000000 ) ) ;
#11042 = VERTEX_POINT ( 'NONE', #15355 ) ;
#11043 = CARTESIAN_POINT ( 'NONE',  ( 0.2233192592356400275, 0.09374999990245759529, -0.3073725909049499494 ) ) ;
#11044 = ORIENTED_EDGE ( 'NONE', *, *, #20955, .F. ) ;
#11045 = CARTESIAN_POINT ( 'NONE',  ( 0.2726353606394136819, 5.081042968642144331, 0.1517956056947933619 ) ) ;
#11046 = CARTESIAN_POINT ( 'NONE',  ( 0.1144950937579611444, 0.2764156081756483641, 0.1820833333333359561 ) ) ;
#11047 = AXIS2_PLACEMENT_3D ( 'NONE', #9638, #13195, #11472 ) ;
#11048 = CARTESIAN_POINT ( 'NONE',  ( 0.1167790944451424368, 4.314666666742532186, 0.2819296736111110424 ) ) ;
#11049 = CARTESIAN_POINT ( 'NONE',  ( -0.2819296736111110979, 5.071611111186976828, -0.1167790944451422980 ) ) ;
#11050 = CARTESIAN_POINT ( 'NONE',  ( 0.3023734573831431405, -0.03492818159268935158, 0.4159249849313371161 ) ) ;
#11051 = CARTESIAN_POINT ( 'NONE',  ( -0.3070831450522693573, 4.225926056666180486, 0.05521187652797088230 ) ) ;
#11052 = CARTESIAN_POINT ( 'NONE',  ( -0.3119999999999999996, 3.939666666666666206, 0.000000000000000000 ) ) ;
#11053 = CARTESIAN_POINT ( 'NONE',  ( -0.3119999999999998885, 4.894527777929509327, 0.1292346314604058410 ) ) ;
#11054 = CARTESIAN_POINT ( 'NONE',  ( -1.726321361862525858E-17, 5.130638888964754507, -0.2819296736111110979 ) ) ;
#11055 = CARTESIAN_POINT ( 'NONE',  ( -0.4366234456863259394, 1.999640111863030478, -2.684082427924094016 ) ) ;
#11056 = ORIENTED_EDGE ( 'NONE', *, *, #8365, .F. ) ;
#11057 = EDGE_CURVE ( 'NONE', #7667, #16613, #18031, .T. ) ;
#11058 = DIRECTION ( 'NONE',  ( -0.000000000000000000, -1.000000000000000000, -0.000000000000000000 ) ) ;
#11059 = CARTESIAN_POINT ( 'NONE',  ( 0.2830627371972649908, 0.03488899866380682641, -0.02971062478493903189 ) ) ;
#11060 = CC_DESIGN_PERSON_AND_ORGANIZATION_ASSIGNMENT ( #4660, #17837, ( #12722 ) ) ;
#11061 = CIRCLE ( 'NONE', #9895, 0.001000000000000003057 ) ;
#11062 = CARTESIAN_POINT ( 'NONE',  ( -0.1306872919485614903, 0.3155070326520293400, 0.2775694444444480324 ) ) ;
#11063 = CARTESIAN_POINT ( 'NONE',  ( 0.2819296736111110979, 5.102861111186976828, -3.452642723725051716E-17 ) ) ;
#11064 = CARTESIAN_POINT ( 'NONE',  ( 0.06335377612981456241, 0.02683051005524446364, 0.3999999999999999667 ) ) ;
#11065 = FACE_OUTER_BOUND ( 'NONE', #9288, .T. ) ;
#11066 = ORIENTED_EDGE ( 'NONE', *, *, #906, .T. ) ;
#11067 = CARTESIAN_POINT ( 'NONE',  ( 0.1993543840281266355, 0.3201388888130222710, 0.1993543840281267465 ) ) ;
#11068 = CARTESIAN_POINT ( 'NONE',  ( 0.1144950937579609085, -0.2764156081756484751, 0.1681944444444469222 ) ) ;
#11069 = CARTESIAN_POINT ( 'NONE',  ( -1.726321361862525858E-17, 4.908416666742532186, -0.2819296736111110979 ) ) ;
#11070 = CARTESIAN_POINT ( 'NONE',  ( 0.3048113794607916205, 4.476554688488221245, -0.07360551287067333692 ) ) ;
#11071 = ORIENTED_EDGE ( 'NONE', *, *, #5219, .F. ) ;
#11072 = CARTESIAN_POINT ( 'NONE',  ( 0.1993543840281266633, 4.832027777853643791, -0.1993543840281266910 ) ) ;
#11073 = FACE_OUTER_BOUND ( 'NONE', #4724, .T. ) ;
#11074 = DIRECTION ( 'NONE',  ( 0.8660254037844382635, 0.000000000000000000, -0.5000000000000004441 ) ) ;
#11075 = FACE_OUTER_BOUND ( 'NONE', #7365, .T. ) ;
#11076 = CARTESIAN_POINT ( 'NONE',  ( -0.3125000000000000000, 1.913510623667739771E-17, 0.3383333333333369830 ) ) ;
#11077 = CARTESIAN_POINT ( 'NONE',  ( -0.3119999999999998885, 4.498694444444443441, 0.1292346314604058410 ) ) ;
#11078 = CARTESIAN_POINT ( 'NONE',  ( 0.2819296736111111534, 3.988277777853643347, 0.1167790944451422563 ) ) ;
#11079 = VECTOR ( 'NONE', #9520, 39.37007874015748143 ) ;
#11080 = FACE_OUTER_BOUND ( 'NONE', #9249, .T. ) ;
#11081 = CARTESIAN_POINT ( 'NONE',  ( 0.3066522881518912169, 4.031597852227386980, -0.05855820888548868286 ) ) ;
#11082 = CARTESIAN_POINT ( 'NONE',  ( 5.731347020009612645E-17, 4.397999999999999687, 0.3119999999999999996 ) ) ;
#11083 = DIRECTION ( 'NONE',  ( -0.000000000000000000, 1.000000000000000000, -0.000000000000000000 ) ) ;
#11084 = ORIENTED_EDGE ( 'NONE', *, *, #23647, .T. ) ;
#11085 = DIRECTION ( 'NONE',  ( 0.000000000000000000, 0.000000000000000000, 1.000000000000000000 ) ) ;
#11086 = EDGE_CURVE ( 'NONE', #13879, #10939, #17060, .T. ) ;
#11087 = CARTESIAN_POINT ( 'NONE',  ( -0.4500000000000003997, -0.2598076211353319009, 0.3779506566538942125 ) ) ;
#11088 = CARTESIAN_POINT ( 'NONE',  ( 0.1954553509668047195, 0.1954553509668046085, 0.1786111111111137462 ) ) ;
#11089 = AXIS2_PLACEMENT_3D ( 'NONE', #13081, #15137, #1962 ) ;
#11090 = DIRECTION ( 'NONE',  ( 0.000000000000000000, 0.8660254037842882724, 0.5000000000002605693 ) ) ;
#11091 = CARTESIAN_POINT ( 'NONE',  ( -0.2495012331031523645, 4.440889594020191566, -0.1917320893305669016 ) ) ;
#11092 = CARTESIAN_POINT ( 'NONE',  ( -0.01294618724694486522, -0.5474118055169125974, 0.04270874187135764027 ) ) ;
#11093 = CARTESIAN_POINT ( 'NONE',  ( 0.1116596296178199860, 0.3116071427596003862, -0.3436530038418508792 ) ) ;
#11094 = CARTESIAN_POINT ( 'NONE',  ( 0.2819296736111110424, 0.3097222221463555303, 0.1167790944451424923 ) ) ;
#11095 = PLANE ( 'NONE',  #15993 ) ;
#11096 = DIRECTION ( 'NONE',  ( -0.000000000000000000, -1.000000000000000000, -0.000000000000000000 ) ) ;
#11097 = CYLINDRICAL_SURFACE ( 'NONE', #24128, 0.3119999999999999996 ) ;
#11098 = CARTESIAN_POINT ( 'NONE',  ( 0.1954553509668046640, -0.1954553509668047195, -0.1061111111111108091 ) ) ;
#11099 = ORIENTED_EDGE ( 'NONE', *, *, #21699, .F. ) ;
#11100 = VERTEX_POINT ( 'NONE', #18649 ) ;
#11101 = DIRECTION ( 'NONE',  ( 0.000000000000000000, 0.000000000000000000, 1.000000000000000000 ) ) ;
#11102 = CARTESIAN_POINT ( 'NONE',  ( 0.4592349292584271825, -0.08929898372139863372, 0.4306178066313481878 ) ) ;
#11103 = LOCAL_TIME ( 21, 9, 13.00000000000000000, #11302 ) ;
#11104 = CARTESIAN_POINT ( 'NONE',  ( 1.910449006669871087E-17, 0.03194444444444410891, -0.3119999999999999996 ) ) ;
#11105 = CARTESIAN_POINT ( 'NONE',  ( 5.178964085587577574E-17, 3.936194444520310309, 0.2819296736111110979 ) ) ;
#11106 = CARTESIAN_POINT ( 'NONE',  ( -0.3613381517857143232, 0.2616071427596003973, -4.425116109941954795E-17 ) ) ;
#11107 = CARTESIAN_POINT ( 'NONE',  ( -0.1993543840281266355, 4.429250000075866112, 0.1993543840281267465 ) ) ;
#11108 = LINE ( 'NONE', #22074, #23652 ) ;
#11109 = ADVANCED_FACE ( 'NONE', ( #7551 ), #11097, .T. ) ;
#11110 = DIRECTION ( 'NONE',  ( 1.000000000000000000, 0.000000000000000000, 0.000000000000000000 ) ) ;
#11111 = ORIENTED_EDGE ( 'NONE', *, *, #5971, .T. ) ;
#11112 = EDGE_CURVE ( 'NONE', #4857, #8682, #3234, .T. ) ;
#11113 = CARTESIAN_POINT ( 'NONE',  ( 0.3236067977499789694, 0.3928571428571427382, 0.2351141009169893659 ) ) ;
#11114 = CARTESIAN_POINT ( 'NONE',  ( 0.1167790944451422702, 5.002166666742531298, -0.2819296736111110424 ) ) ;
#11115 = AXIS2_PLACEMENT_3D ( 'NONE', #11455, #6071, #9866 ) ;
#11116 = CARTESIAN_POINT ( 'NONE',  ( -0.1507786080989017841, 5.147423691745167673, -0.2635463223593010884 ) ) ;
#11117 = EDGE_CURVE ( 'NONE', #18827, #5903, #15238, .T. ) ;
#11118 = CARTESIAN_POINT ( 'NONE',  ( -0.3119999999999999996, 4.991749999999998799, -0.1292346314604056468 ) ) ;
#11119 = CC_DESIGN_SECURITY_CLASSIFICATION ( #13854, ( #17744 ) ) ;
#11120 = CARTESIAN_POINT ( 'NONE',  ( -0.2819296736111110979, 4.682722222298087544, -0.1167790944451422980 ) ) ;
#11121 = DATE_AND_TIME ( #12967, #11544 ) ;
#11122 = CARTESIAN_POINT ( 'NONE',  ( -0.4678838860311506087, 0.2663291305467040404, 0.05893128447555430471 ) ) ;
#11123 = CARTESIAN_POINT ( 'NONE',  ( 0.000000000000000000, 3.700000000000000622, 0.000000000000000000 ) ) ;
#11124 = CARTESIAN_POINT ( 'NONE',  ( -0.1167790944451424368, 0.5319444443685777957, 0.2819296736111110424 ) ) ;
#11125 = EDGE_LOOP ( 'NONE', ( #7342, #17646, #19538, #8095 ) ) ;
#11126 = ORIENTED_EDGE ( 'NONE', *, *, #22890, .T. ) ;
#11127 = CARTESIAN_POINT ( 'NONE',  ( -0.1993543840281266633, 0.2368055554796889006, -0.1993543840281266910 ) ) ;
#11128 = CARTESIAN_POINT ( 'NONE',  ( 0.3125000000000000000, 3.827021247335477694E-17, 1.326383476483184332 ) ) ;
#11129 = CARTESIAN_POINT ( 'NONE',  ( -0.5116234456863466562, 3.856336430858469555, 2.549370209580444691 ) ) ;
#11130 = AXIS2_PLACEMENT_3D ( 'NONE', #14708, #1408, #3588 ) ;
#11131 = CARTESIAN_POINT ( 'NONE',  ( 0.3999999999999999667, 0.2535714285714285032, 0.1299678784931626307 ) ) ;
#11132 = CARTESIAN_POINT ( 'NONE',  ( -0.2230971623002953874, 0.2230971623002954152, -0.05576388888888837714 ) ) ;
#11133 = FACE_OUTER_BOUND ( 'NONE', #13877, .T. ) ;
#11134 = CARTESIAN_POINT ( 'NONE',  ( -0.1235199187034025786, 3.880721340484976078, -0.2869016881843655109 ) ) ;
#11135 = CARTESIAN_POINT ( 'NONE',  ( 0.2819296736111110979, 0.3131944443685777957, 0.000000000000000000 ) ) ;
#11136 = CARTESIAN_POINT ( 'NONE',  ( 1.726321361862525858E-17, 0.04930555547968892144, -0.2819296736111110979 ) ) ;
#11137 = CARTESIAN_POINT ( 'NONE',  ( -0.1993543840281266910, 4.582027777853643791, -0.1993543840281266910 ) ) ;
#11138 = CARTESIAN_POINT ( 'NONE',  ( 0.2472135954999579721, 0.1160714283763437799, -0.3402603233408159622 ) ) ;
#11139 = CARTESIAN_POINT ( 'NONE',  ( 0.04183867695277764670, 4.542642517705186123, -0.3092924480017552047 ) ) ;
#11140 = CARTESIAN_POINT ( 'NONE',  ( -0.2819296736111110424, 5.036888888964754507, 0.1167790944451424923 ) ) ;
#11141 = CARTESIAN_POINT ( 'NONE',  ( -0.2819296736111110424, 4.411888888964754507, 0.1167790944451424923 ) ) ;
#11142 = CARTESIAN_POINT ( 'NONE',  ( 0.1307108517531567482, 3.742116710486879327, 0.2841574553316881246 ) ) ;
#11143 = LOCAL_TIME ( 21, 9, 13.00000000000000000, #11606 ) ;
#11144 = CARTESIAN_POINT ( 'NONE',  ( -0.009374999999999951081, -0.5358532185916218271, 0.4425000000000000044 ) ) ;
#11145 = CARTESIAN_POINT ( 'NONE',  ( -0.3116633497045768197, 3.673292956572201451, -0.09499999999999995948 ) ) ;
#11146 = CARTESIAN_POINT ( 'NONE',  ( 0.3119999999999999996, 4.141055555707287894, -3.820898013339742174E-17 ) ) ;
#11147 = CARTESIAN_POINT ( 'NONE',  ( -0.2819296736111110424, 4.425777777853642903, 0.1167790944451424923 ) ) ;
#11148 = CARTESIAN_POINT ( 'NONE',  ( -0.3291860208797072751, 0.3512102395969135538, 0.4108348780186336091 ) ) ;
#11149 = ORIENTED_EDGE ( 'NONE', *, *, #14566, .F. ) ;
#11150 = VECTOR ( 'NONE', #18836, 39.37007874015748143 ) ;
#11151 = EDGE_CURVE ( 'NONE', #21943, #17107, #16939, .T. ) ;
#11152 = ORIENTED_EDGE ( 'NONE', *, *, #5440, .T. ) ;
#11153 = VERTEX_POINT ( 'NONE', #24122 ) ;
#11154 = PERSON_AND_ORGANIZATION ( #15518, #2538 ) ;
#11155 = CARTESIAN_POINT ( 'NONE',  ( 0.4570242136016680612, -0.2774028246161726607, 0.04874733047934382002 ) ) ;
#11156 = CARTESIAN_POINT ( 'NONE',  ( -0.09380593400082881672, 0.03242967361111052244, 0.2658661084243340578 ) ) ;
#11157 = DIRECTION ( 'NONE',  ( -0.000000000000000000, -1.000000000000000000, 0.000000000000000000 ) ) ;
#11158 = APPROVAL_PERSON_ORGANIZATION ( #18669, #4198, #20503 ) ;
#11159 = ORIENTED_EDGE ( 'NONE', *, *, #18097, .F. ) ;
#11160 = CARTESIAN_POINT ( 'NONE',  ( 0.3119999999999999996, 0.5701388887371559022, -0.1292346314604056468 ) ) ;
#11161 = VERTEX_POINT ( 'NONE', #19016 ) ;
#11162 = CARTESIAN_POINT ( 'NONE',  ( 1.573500000000000343, 2.683750000000000746, -1.006250000000000533 ) ) ;
#11163 = CARTESIAN_POINT ( 'NONE',  ( -0.2348053674301955052, 3.718086869336296729, -0.2057751470050347142 ) ) ;
#11164 = CARTESIAN_POINT ( 'NONE',  ( 2.936000000000000387, 0.000000000000000000, -2.541000000000000369 ) ) ;
#11165 = CARTESIAN_POINT ( 'NONE',  ( 0.000000000000000000, 0.9099999999999988098, 0.7500000000000001110 ) ) ;
#11166 = ORIENTED_EDGE ( 'NONE', *, *, #11276, .F. ) ;
#11167 = CARTESIAN_POINT ( 'NONE',  ( 0.3613381517857143232, 0.07946428561674330482, 0.1174058825155741975 ) ) ;
#11168 = CIRCLE ( 'NONE', #20883, 0.01874999999999999237 ) ;
#11169 = VERTEX_POINT ( 'NONE', #13415 ) ;
#11170 = CARTESIAN_POINT ( 'NONE',  ( 0.1484364568374648974, 5.095438198970610344, -0.2736806903221176701 ) ) ;
#11171 = CARTESIAN_POINT ( 'NONE',  ( -3.385114897866767815E-17, -0.2764156081756484196, 0.2133333333333362336 ) ) ;
#11172 = CARTESIAN_POINT ( 'NONE',  ( -0.1993543840281266355, 4.248694444520309865, 0.1993543840281267465 ) ) ;
#11173 = CARTESIAN_POINT ( 'NONE',  ( 0.2819296736111110979, 5.106333333409199149, -0.1167790944451423396 ) ) ;
#11174 = CARTESIAN_POINT ( 'NONE',  ( 0.000000000000000000, 0.000000000000000000, 0.000000000000000000 ) ) ;
#11175 = PLANE ( 'NONE',  #16275 ) ;
#11176 = CARTESIAN_POINT ( 'NONE',  ( -0.1292346314604056745, 3.818138888888887639, -0.3119999999999999996 ) ) ;
#11177 = CARTESIAN_POINT ( 'NONE',  ( -0.3119999999999999996, 4.724388889040620931, 0.000000000000000000 ) ) ;
#11178 = CARTESIAN_POINT ( 'NONE',  ( 0.1607903964422072729, 4.798635960660796229, 0.2688681601943798682 ) ) ;
#11179 = CARTESIAN_POINT ( 'NONE',  ( 0.3950000000000000178, 2.665000000000000036, -1.966000000000000192 ) ) ;
#11180 = ORIENTED_EDGE ( 'NONE', *, *, #5457, .T. ) ;
#11181 = CARTESIAN_POINT ( 'NONE',  ( -0.2923287055106771337, 0.1794642856167432687, 0.2123892367102619971 ) ) ;
#11182 = CARTESIAN_POINT ( 'NONE',  ( 0.1515256109559866837, 0.04002383242775373051, -0.2469710999841635557 ) ) ;
#11183 = CIRCLE ( 'NONE', #659, 0.3125000000000001665 ) ;
#11184 = ORIENTED_EDGE ( 'NONE', *, *, #4050, .T. ) ;
#11185 = PERSON_AND_ORGANIZATION ( #15518, #2538 ) ;
#11186 = CARTESIAN_POINT ( 'NONE',  ( 0.3155070326520292845, -5.795770164686806123E-17, 0.3157638888888927853 ) ) ;
#11187 = CARTESIAN_POINT ( 'NONE',  ( 0.1993543840281267465, 5.095916666742532186, 0.1993543840281266633 ) ) ;
#11188 = CARTESIAN_POINT ( 'NONE',  ( 0.3107848814624034617, -0.3618341423928899125, 0.4134938258000521172 ) ) ;
#11189 = DIRECTION ( 'NONE',  ( -0.4995222938423191095, -0.04370253788966848435, 0.8651979924482661177 ) ) ;
#11190 = CARTESIAN_POINT ( 'NONE',  ( -0.1167790944451422702, 0.1777777777019111938, -0.2819296736111110979 ) ) ;
#11191 = CARTESIAN_POINT ( 'NONE',  ( -0.1144950937579609779, 0.2764156081756484196, 0.3070833333333369275 ) ) ;
#11192 = CARTESIAN_POINT ( 'NONE',  ( 0.2819296736111110979, 4.894527777853643791, -3.452642723725051716E-17 ) ) ;
#11193 = CARTESIAN_POINT ( 'NONE',  ( 0.2594935920934202112, 4.479718426223786132, -0.1748956054335727706 ) ) ;
#11194 = CARTESIAN_POINT ( 'NONE',  ( -0.1167790944451423535, 4.918833333409199149, 0.2819296736111110424 ) ) ;
#11195 = CYLINDRICAL_SURFACE ( 'NONE', #2512, 0.3119999999999999996 ) ;
#11196 = CARTESIAN_POINT ( 'NONE',  ( -5.731347020009612645E-17, 0.4972222220704892726, 0.3119999999999999996 ) ) ;
#11197 = CARTESIAN_POINT ( 'NONE',  ( 0.2206173157302027954, 4.585499999999999687, -0.2206173157302028232 ) ) ;
#11198 = CYLINDRICAL_SURFACE ( 'NONE', #15103, 0.3125000000000000555 ) ;
#11199 = CARTESIAN_POINT ( 'NONE',  ( -0.1292346314604056745, 4.429249999999999687, -0.3119999999999999996 ) ) ;
#11200 = CARTESIAN_POINT ( 'NONE',  ( -0.1993543840281266355, 4.026472222298087544, 0.1993543840281267465 ) ) ;
#11201 = LINE ( 'NONE', #18631, #12060 ) ;
#11202 = SHAPE_REPRESENTATION ( 'Aloris-BXA-Wedge-R', ( #9127 ), #5239 ) ;
#11203 = CARTESIAN_POINT ( 'NONE',  ( 2.500728763858895135E-17, 6.000000000000000888, 0.2041999999999999926 ) ) ;
#11204 = CARTESIAN_POINT ( 'NONE',  ( -0.03716597311884842908, 3.737241779597674896, 0.3101143021802981181 ) ) ;
#11205 = VERTEX_POINT ( 'NONE', #16703 ) ;
#11206 = CARTESIAN_POINT ( 'NONE',  ( 0.3102328094856748320, 4.584584709764821575, 0.03329712396315245154 ) ) ;
#11207 = EDGE_LOOP ( 'NONE', ( #15436, #18393, #6847, #19416 ) ) ;
#11208 = CARTESIAN_POINT ( 'NONE',  ( -0.04615996209784192089, -0.5146154108223025547, 0.3902123106865083013 ) ) ;
#11209 = DIRECTION ( 'NONE',  ( 0.000000000000000000, 0.000000000000000000, -1.000000000000000000 ) ) ;
#11210 = CARTESIAN_POINT ( 'NONE',  ( 0.1954553509668046640, -0.1954553509668047195, 0.2758333333333367055 ) ) ;
#11211 = DIRECTION ( 'NONE',  ( -0.000000000000000000, -1.000000000000000000, -0.000000000000000000 ) ) ;
#11212 = CARTESIAN_POINT ( 'NONE',  ( -0.04082748817735452201, 4.459360436992971799, 0.3119999991102669901 ) ) ;
#11213 = ORIENTED_EDGE ( 'NONE', *, *, #15292, .F. ) ;
#11214 = EDGE_CURVE ( 'NONE', #15369, #23837, #23139, .T. ) ;
#11215 = CARTESIAN_POINT ( 'NONE',  ( -0.1116596296178200276, 0.2044642856167432909, 0.3436530038418508792 ) ) ;
#11216 = CARTESIAN_POINT ( 'NONE',  ( 0.1167790944451423257, 0.2680555554796889561, -0.2819296736111110424 ) ) ;
#11217 = CARTESIAN_POINT ( 'NONE',  ( 0.08089722802934988521, 3.874934476269974670, -0.3020209484956946078 ) ) ;
#11218 = DIRECTION ( 'NONE',  ( 0.000000000000000000, 0.000000000000000000, -1.000000000000000000 ) ) ;
#11219 = EDGE_CURVE ( 'NONE', #8072, #10945, #2548, .T. ) ;
#11220 = CARTESIAN_POINT ( 'NONE',  ( -0.2209708691207961373, -0.2209708691207961095, 0.06750000000000151712 ) ) ;
#11221 = CARTESIAN_POINT ( 'NONE',  ( 0.1144950937579611444, 0.2764156081756483641, 0.02236111111111246247 ) ) ;
#11222 = ORIENTED_EDGE ( 'NONE', *, *, #2134, .T. ) ;
#11223 = DIRECTION ( 'NONE',  ( -0.000000000000000000, -1.000000000000000000, -0.000000000000000000 ) ) ;
#11224 = CARTESIAN_POINT ( 'NONE',  ( 0.4687500000000002776, 0.1103509067785291842, 0.4107148665556337175 ) ) ;
#11225 = CARTESIAN_POINT ( 'NONE',  ( 0.2206173157302028232, 0.08055555555555521385, -0.2206173157302028232 ) ) ;
#11226 = CARTESIAN_POINT ( 'NONE',  ( -0.1292346314604056745, 5.151472222222222008, -0.3119999999999999996 ) ) ;
#11227 = CARTESIAN_POINT ( 'NONE',  ( 0.3613381517857143232, 0.3008928570453147100, -0.1174058825155740587 ) ) ;
#11228 = ADVANCED_FACE ( 'NONE', ( #8142 ), #13891, .F. ) ;
#11229 = CARTESIAN_POINT ( 'NONE',  ( 0.1993543840281266633, 4.290361111186976828, -0.1993543840281266910 ) ) ;
#11230 = CARTESIAN_POINT ( 'NONE',  ( 0.000000000000000000, 5.384999999999999787, -0.3119999999999999996 ) ) ;
#11231 = CARTESIAN_POINT ( 'NONE',  ( 0.3311950453211457424, -4.100712535614406822E-18, -0.1463848030125310673 ) ) ;
#11232 = VERTEX_POINT ( 'NONE', #10116 ) ;
#11233 = VERTEX_POINT ( 'NONE', #12071 ) ;
#11234 = CIRCLE ( 'NONE', #13197, 0.7650000000000000133 ) ;
#11235 = CARTESIAN_POINT ( 'NONE',  ( 0.2348386186658658059, 4.356861530419343431, 0.2064237969327863131 ) ) ;
#11236 = CARTESIAN_POINT ( 'NONE',  ( -0.1993543840281266910, 5.012583333409199149, -0.1993543840281266910 ) ) ;
#11237 = CARTESIAN_POINT ( 'NONE',  ( 0.0005099541946469743911, 2.690509954194647335, -0.8851373192811128332 ) ) ;
#11238 = LENGTH_MEASURE_WITH_UNIT ( LENGTH_MEASURE( 0.02539999999999999897 ), #22318 );
#11239 = CARTESIAN_POINT ( 'NONE',  ( 0.03587150718080267531, 3.709525392854851056, -0.3100612275418990760 ) ) ;
#11240 = CYLINDRICAL_SURFACE ( 'NONE', #8348, 0.3119999999999999996 ) ;
#11241 = CARTESIAN_POINT ( 'NONE',  ( -0.2819296736111110424, 4.689666666742532186, 0.1167790944451424923 ) ) ;
#11242 = APPROVAL_ROLE ( '' ) ;
#11243 = LINE ( 'NONE', #9408, #15231 ) ;
#11244 = CARTESIAN_POINT ( 'NONE',  ( -0.09380593400082881672, 0.03242967361111052244, 0.2658661084243340578 ) ) ;
#11245 = CARTESIAN_POINT ( 'NONE',  ( -0.1993543840281266633, 0.5701388888130222155, -0.1993543840281266910 ) ) ;
#11246 = ADVANCED_FACE ( 'NONE', ( #714 ), #17541, .T. ) ;
#11248 = VERTEX_POINT ( 'NONE', #6554 ) ;
#11247 = VECTOR ( 'NONE', #13687, 39.37007874015748143 ) ;
#11249 = ORIENTED_EDGE ( 'NONE', *, *, #11314, .F. ) ;
#11250 = CARTESIAN_POINT ( 'NONE',  ( -0.2819296736111110979, 0.2993055554796889561, -3.452642723725051716E-17 ) ) ;
#11251 = CARTESIAN_POINT ( 'NONE',  ( 3.073863465859856523E-17, 5.501232050807569607, 0.2510000000000000009 ) ) ;
#11252 = CYLINDRICAL_SURFACE ( 'NONE', #12121, 0.3119999999999999996 ) ;
#11253 = CARTESIAN_POINT ( 'NONE',  ( -0.4000000000000000222, 0.1535714285714285254, 0.1299678784931624920 ) ) ;
#11254 = CARTESIAN_POINT ( 'NONE',  ( -3.863846776457871776E-17, -0.3155070326520292845, -0.09048611111111086458 ) ) ;
#11255 = CARTESIAN_POINT ( 'NONE',  ( 0.4687500000000002776, -0.2598076211353317344, 0.3779506566538943235 ) ) ;
#11256 = CARTESIAN_POINT ( 'NONE',  ( 0.3950000000000000178, 2.665000000000000036, -2.591000000000000192 ) ) ;
#11257 = CARTESIAN_POINT ( 'NONE',  ( -0.2819296736111110979, 0.2819444443685778512, -0.1167790944451423396 ) ) ;
#11258 = CARTESIAN_POINT ( 'NONE',  ( 0.1993543840281267465, 4.332027777853642903, 0.1993543840281266633 ) ) ;
#11259 = CARTESIAN_POINT ( 'NONE',  ( -0.3236067977499789694, 0.1339285712334866152, -0.2351141009169893104 ) ) ;
#11260 = EDGE_CURVE ( 'NONE', #280, #8797, #2928, .T. ) ;
#11261 = CARTESIAN_POINT ( 'NONE',  ( 5.178964085587577574E-17, 5.047305555631421470, 0.2819296736111110979 ) ) ;
#11262 = CARTESIAN_POINT ( 'NONE',  ( -0.1993543840281266910, 4.401472222298088433, -0.1993543840281266910 ) ) ;
#11263 = DIRECTION ( 'NONE',  ( 0.000000000000000000, -1.000000000000000000, 0.000000000000000000 ) ) ;
#11264 = ORIENTED_EDGE ( 'NONE', *, *, #2968, .F. ) ;
#11265 = CARTESIAN_POINT ( 'NONE',  ( -0.2721215285213482993, 0.3841564396211271104, 0.07944889038199838549 ) ) ;
#11266 = CARTESIAN_POINT ( 'NONE',  ( 0.3119999999999999996, 4.085500000151732536, -3.820898013339742174E-17 ) ) ;
#11267 = DIRECTION ( 'NONE',  ( -0.000000000000000000, 1.000000000000000000, -0.000000000000000000 ) ) ;
#11268 = AXIS2_PLACEMENT_3D ( 'NONE', #8622, #20081, #16063 ) ;
#11269 = DIRECTION ( 'NONE',  ( -0.000000000000000000, -1.000000000000000000, -0.000000000000000000 ) ) ;
#11270 = ORIENTED_EDGE ( 'NONE', *, *, #8731, .F. ) ;
#11271 = PERSON_AND_ORGANIZATION_ROLE ( 'creator' ) ;
#11272 = CARTESIAN_POINT ( 'NONE',  ( -0.1374632086698537592, 4.845340413058586648, 0.2800857552099924042 ) ) ;
#11273 = PLANE ( 'NONE',  #12412 ) ;
#11274 = ORIENTED_EDGE ( 'NONE', *, *, #10680, .F. ) ;
#11275 = CARTESIAN_POINT ( 'NONE',  ( 0.1292346314604056745, 0.4104166665149336923, -0.3119999999999999996 ) ) ;
#11276 = EDGE_CURVE ( 'NONE', #70, #5752, #11633, .T. ) ;
#11277 = ADVANCED_FACE ( 'NONE', ( #21437 ), #13770, .F. ) ;
#11278 = EDGE_LOOP ( 'NONE', ( #10515, #4804, #1283, #17984 ) ) ;
#11279 = LINE ( 'NONE', #18348, #16422 ) ;
#11280 = CARTESIAN_POINT ( 'NONE',  ( 0.2515573277093725024, 4.746441417219358527, 0.1886560052811415422 ) ) ;
#11281 = CARTESIAN_POINT ( 'NONE',  ( -0.1116596296178200276, -0.02767857152611381821, 0.3436530038418508792 ) ) ;
#11282 = CARTESIAN_POINT ( 'NONE',  ( 1.364852645245658621E-07, 4.377166663151471404, -0.3119999999999701346 ) ) ;
#11283 = ORIENTED_EDGE ( 'NONE', *, *, #8397, .T. ) ;
#11284 = CARTESIAN_POINT ( 'NONE',  ( -0.2923287055106771337, 0.1116071427596004445, -0.2123892367102620804 ) ) ;
#11285 = AXIS2_PLACEMENT_3D ( 'NONE', #17173, #13290, #11576 ) ;
#11286 = ORIENTED_EDGE ( 'NONE', *, *, #20352, .T. ) ;
#11287 = CARTESIAN_POINT ( 'NONE',  ( 0.000000000000000000, 0.000000000000000000, 0.000000000000000000 ) ) ;
#11288 = CARTESIAN_POINT ( 'NONE',  ( -0.3127085332352448899, 4.668742369690864535, -0.005568702923292533601 ) ) ;
#11289 = EDGE_CURVE ( 'NONE', #14698, #15146, #17193, .T. ) ;
#11290 = CARTESIAN_POINT ( 'NONE',  ( 0.2819296736111110979, 4.210500000075865223, 0.1167790944451422425 ) ) ;
#11291 = CARTESIAN_POINT ( 'NONE',  ( 0.1975560007912697535, -0.2122688852239507096, 0.4011227751864958058 ) ) ;
#11292 = CARTESIAN_POINT ( 'NONE',  ( 0.08367472778091819552, -0.4929562507565927731, 0.07813238993955244627 ) ) ;
#11293 = CARTESIAN_POINT ( 'NONE',  ( -0.2206173157302028232, 3.821611111111110404, -0.2206173157302028232 ) ) ;
#11294 = CARTESIAN_POINT ( 'NONE',  ( 0.2206173157302027954, 4.703555555707287894, -0.2206173157302028232 ) ) ;
#11295 = CARTESIAN_POINT ( 'NONE',  ( 0.3080665527274119575, 4.806319477209046731, 0.05048669183540833300 ) ) ;
#11296 = DIRECTION ( 'NONE',  ( -1.000000000000000000, -0.000000000000000000, -0.000000000000000000 ) ) ;
#11297 = CARTESIAN_POINT ( 'NONE',  ( 0.2923287055106771337, 0.2151785713310289949, -0.2123892367102620249 ) ) ;
#11298 = AXIS2_PLACEMENT_3D ( 'NONE', #3048, #2803, #1097 ) ;
#11299 = CARTESIAN_POINT ( 'NONE',  ( -0.01971715691147114813, 0.06040120350305807490, 0.3099012035031042944 ) ) ;
#11300 = AXIS2_PLACEMENT_3D ( 'NONE', #13578, #4284, #2468 ) ;
#11301 = EDGE_LOOP ( 'NONE', ( #5412, #21452, #2769, #13497 ) ) ;
#11302 = COORDINATED_UNIVERSAL_TIME_OFFSET ( 0, 0, .AHEAD. ) ;
#11303 = CARTESIAN_POINT ( 'NONE',  ( 0.4723638629038580117, 0.2802187124228171511, 0.04193801346286276516 ) ) ;
#11304 = CARTESIAN_POINT ( 'NONE',  ( 0.1167790944451424368, 5.092444444520309865, 0.2819296736111110424 ) ) ;
#11305 = CARTESIAN_POINT ( 'NONE',  ( -0.1993543840281266355, 3.762583333409198705, 0.1993543840281267465 ) ) ;
#11306 = FACE_OUTER_BOUND ( 'NONE', #12512, .T. ) ;
#11307 = DIRECTION ( 'NONE',  ( 6.123233995739957225E-17, 0.8660254037842882724, -0.5000000000002605693 ) ) ;
#11308 = CARTESIAN_POINT ( 'NONE',  ( 0.1144950937579611444, 0.2764156081756483641, -0.04013888888888803019 ) ) ;
#11309 = CARTESIAN_POINT ( 'NONE',  ( 0.2819296736111110979, 0.4416666665908000611, -0.1167790944451422980 ) ) ;
#11310 = CARTESIAN_POINT ( 'NONE',  ( 0.1954553509668046640, -0.1954553509668047195, 0.1716666666666691599 ) ) ;
#11311 = EDGE_CURVE ( 'NONE', #17737, #4761, #21060, .T. ) ;
#11312 = CARTESIAN_POINT ( 'NONE',  ( -0.2819296736111110424, 4.918833333409199149, -0.1167790944451423119 ) ) ;
#11313 = CARTESIAN_POINT ( 'NONE',  ( -0.003278813451167537571, -0.5383665848074061788, 0.05892894635879412230 ) ) ;
#11314 = EDGE_CURVE ( 'NONE', #5711, #5067, #12671, .T. ) ;
#11315 = CARTESIAN_POINT ( 'NONE',  ( 0.1167790944451424368, 4.814666666742533074, 0.2819296736111110424 ) ) ;
#11316 = AXIS2_PLACEMENT_3D ( 'NONE', #2670, #17545, #9633 ) ;
#11317 = CARTESIAN_POINT ( 'NONE',  ( 0.01223391761890406035, 4.876836776912257143, -0.3117956601136203099 ) ) ;
#11318 = LINE ( 'NONE', #14745, #20731 ) ;
#11319 = CARTESIAN_POINT ( 'NONE',  ( 0.4620753182980354423, 0.2744865679600219099, 0.05975678175779888801 ) ) ;
#11320 = CARTESIAN_POINT ( 'NONE',  ( 0.1292346314604056190, 4.477861111111110404, -0.3119999999999999996 ) ) ;
#11321 = VECTOR ( 'NONE', #20391, 39.37007874015748143 ) ;
#11322 = CARTESIAN_POINT ( 'NONE',  ( 0.1797085267211815662, 3.721720965436318362, -0.2172307213220433242 ) ) ;
#11323 = LINE ( 'NONE', #8213, #12844 ) ;
#11324 = CARTESIAN_POINT ( 'NONE',  ( -0.3119999999999999996, 3.991749999999999243, -0.1292346314604056468 ) ) ;
#11325 = CARTESIAN_POINT ( 'NONE',  ( -0.1051149507764515267, 3.735250598783638409, 0.2937598854384353420 ) ) ;
#11326 = CARTESIAN_POINT ( 'NONE',  ( 0.3108826220787605510, 4.584778751626606308, 0.02638173060821461663 ) ) ;
#11327 = ORIENTED_EDGE ( 'NONE', *, *, #17962, .F. ) ;
#11328 = CARTESIAN_POINT ( 'NONE',  ( -0.2926395827916415948, 4.110145192664806935, -0.1098333424203642578 ) ) ;
#11329 = AXIS2_PLACEMENT_3D ( 'NONE', #16462, #3648, #5725 ) ;
#11330 = CARTESIAN_POINT ( 'NONE',  ( -0.1306872919485614903, 0.3155070326520293400, -0.1113194444444439435 ) ) ;
#11331 = AXIS2_PLACEMENT_3D ( 'NONE', #18633, #5823, #7537 ) ;
#11332 = CARTESIAN_POINT ( 'NONE',  ( 3.820898013339742174E-17, 5.384999999999999787, 0.3119999999999999996 ) ) ;
#11333 = CARTESIAN_POINT ( 'NONE',  ( 0.2880336597100306428, 5.149313696340753310, -0.09459580602892668499 ) ) ;
#11335 = VERTEX_POINT ( 'NONE', #3501 ) ;
#11334 = CC_DESIGN_DATE_AND_TIME_ASSIGNMENT ( #22352, #3580, ( #13854 ) ) ;
#11336 = CARTESIAN_POINT ( 'NONE',  ( -0.2233192592356399442, 0.3937499999024575148, -0.3073725909049500049 ) ) ;
#11337 = CARTESIAN_POINT ( 'NONE',  ( -0.1993543840281266633, 0.3340277777019111660, -0.1993543840281266910 ) ) ;
#11338 = FACE_OUTER_BOUND ( 'NONE', #22812, .T. ) ;
#11339 = CARTESIAN_POINT ( 'NONE',  ( 0.1580470504400612042, 0.2183455552519602272, -1.222587402392238065 ) ) ;
#11340 = CARTESIAN_POINT ( 'NONE',  ( 0.2156887100776809230, 0.4167379425407623517, 0.4181572966874575470 ) ) ;
#11341 = CARTESIAN_POINT ( 'NONE',  ( -0.1144950937579609779, 0.2764156081756484196, 0.08486111111111295513 ) ) ;
#11342 =( BOUNDED_CURVE ( )  B_SPLINE_CURVE ( 2, ( #18748, #9240, #24103, #20218, #3624, #10958, #2044, #20336, #7294 ),
 .UNSPECIFIED., .F., .F. ) 
 B_SPLINE_CURVE_WITH_KNOTS ( ( 3, 2, 2, 2, 3 ),
 ( 0.1339285714285714246, 0.1383928571428570675, 0.1428571428571426827, 0.1473214285714283533, 0.1517857142857139685 ),
 .UNSPECIFIED. ) 
 CURVE ( )  GEOMETRIC_REPRESENTATION_ITEM ( )  RATIONAL_B_SPLINE_CURVE ( ( 1.000000000000000000, 0.9238795325112867385, 1.000000000000000000, 0.9238795325112867385, 1.000000000000000000, 0.9238795325112867385, 1.000000000000000000, 0.9238795325112919565, 0.9999999999999947820 ) ) 
 REPRESENTATION_ITEM ( '' )  );
#11343 = CARTESIAN_POINT ( 'NONE',  ( 1.910449006669871087E-17, 0.6361111109593781121, -0.3119999999999999996 ) ) ;
#11344 =( BOUNDED_CURVE ( )  B_SPLINE_CURVE ( 2, ( #9018, #18164, #23752, #14512, #5226, #23871, #22983 ),
 .UNSPECIFIED., .F., .F. ) 
 B_SPLINE_CURVE_WITH_KNOTS ( ( 3, 2, 2, 3 ),
 ( 0.07711994006981462424, 0.08333333333333332871, 0.09375000000000000000, 0.1041666666666666713 ),
 .UNSPECIFIED. ) 
 CURVE ( )  GEOMETRIC_REPRESENTATION_ITEM ( )  RATIONAL_B_SPLINE_CURVE ( ( 0.9633570533295530147, 0.9545952256086144283, 1.000000000000000000, 0.9238795325112867385, 1.000000000000000000, 0.9238795325112867385, 1.000000000000000000 ) ) 
 REPRESENTATION_ITEM ( '' )  );
#11345 = CARTESIAN_POINT ( 'NONE',  ( 0.4687500000000002220, -0.2630787017013381246, 0.3892820121258429023 ) ) ;
#11346 = CARTESIAN_POINT ( 'NONE',  ( 0.2206173157302027676, 0.2888888888888885287, 0.2206173157302028787 ) ) ;
#11347 = CARTESIAN_POINT ( 'NONE',  ( 0.3119999999999999996, 5.245222222222222008, -3.820898013339742174E-17 ) ) ;
#11348 = CARTESIAN_POINT ( 'NONE',  ( -0.1167790944451423257, 4.300777777853642903, -0.2819296736111110424 ) ) ;
#11349 = CARTESIAN_POINT ( 'NONE',  ( 0.3125000000000000000, -5.740531871003217465E-17, 0.03972222222222387966 ) ) ;
#11350 = CARTESIAN_POINT ( 'NONE',  ( 0.4749999999999999778, 3.575000000000000622, 0.09499999999999998723 ) ) ;
#11351 = ADVANCED_FACE ( 'NONE', ( #14242 ), #10699, .T. ) ;
#11352 = ORIENTED_EDGE ( 'NONE', *, *, #23018, .F. ) ;
#11353 = VERTEX_POINT ( 'NONE', #18967 ) ;
#11354 = CARTESIAN_POINT ( 'NONE',  ( 0.08808798601665612793, 3.066692553488282957, 3.256612888476066558 ) ) ;
#11355 = CARTESIAN_POINT ( 'NONE',  ( 0.1993543840281267465, 4.984805555631420582, 0.1993543840281266633 ) ) ;
#11356 = CARTESIAN_POINT ( 'NONE',  ( -0.2209708691207961095, 0.2209708691207961373, 0.005000000000001404363 ) ) ;
#11357 = ADVANCED_FACE ( 'NONE', ( #2264 ), #14720, .F. ) ;
#11358 =( LENGTH_UNIT ( ) NAMED_UNIT ( * ) SI_UNIT ( $, .METRE. ) );
#11359 = CARTESIAN_POINT ( 'NONE',  ( -0.009375000000000190473, 0.5358532185916217161, 0.06112444011295373181 ) ) ;
#11360 = CARTESIAN_POINT ( 'NONE',  ( -0.3120000000000000551, 0.2159722222222218713, 0.1292346314604056190 ) ) ;
#11361 = CARTESIAN_POINT ( 'NONE',  ( 0.2819296736111110979, 4.661888888964753619, -0.1167790944451423396 ) ) ;
#11362 = COORDINATED_UNIVERSAL_TIME_OFFSET ( 0, 0, .AHEAD. ) ;
#11363 = CC_DESIGN_PERSON_AND_ORGANIZATION_ASSIGNMENT ( #14540, #20019, ( #7632 ) ) ;
#11364 = CARTESIAN_POINT ( 'NONE',  ( 0.000000000000000000, 5.384999999999999787, 1.910449006669871087E-17 ) ) ;
#11365 = CARTESIAN_POINT ( 'NONE',  ( 0.1954553509668046640, -0.1954553509668047195, 0.005000000000001192726 ) ) ;
#11366 = CARTESIAN_POINT ( 'NONE',  ( 0.1167790944451423535, 0.5944444443685777957, 0.2819296736111110424 ) ) ;
#11367 = VERTEX_POINT ( 'NONE', #4562 ) ;
#11368 = CARTESIAN_POINT ( 'NONE',  ( -0.2819296736111110979, 0.1916666665908000333, 0.1167790944451422425 ) ) ;
#11369 = DIRECTION ( 'NONE',  ( -0.000000000000000000, -1.000000000000000000, -0.000000000000000000 ) ) ;
#11370 = CARTESIAN_POINT ( 'NONE',  ( 3.429644138441397019E-17, 0.000000000000000000, -0.2495000000000007212 ) ) ;
#11371 = CARTESIAN_POINT ( 'NONE',  ( -0.3236067977499790249, 0.1571428571428570564, 0.2351141009169892271 ) ) ;
#11372 = CARTESIAN_POINT ( 'NONE',  ( -0.1306872919485615459, -0.3155070326520293400, -0.03840277777777712648 ) ) ;
#11373 = CARTESIAN_POINT ( 'NONE',  ( -0.1961921601747129984, -0.4279942808755098360, 0.09139393128960894563 ) ) ;
#11374 = CARTESIAN_POINT ( 'NONE',  ( -0.4687500000000003886, -0.2706329386826373806, 0.4425000000000000044 ) ) ;
#11375 = CARTESIAN_POINT ( 'NONE',  ( -0.1167790944451422702, 0.2749999999241334314, -0.2819296736111110979 ) ) ;
#11376 = CARTESIAN_POINT ( 'NONE',  ( -0.1993543840281267465, 0.07013888881302225708, 0.1993543840281266633 ) ) ;
#11377 = CARTESIAN_POINT ( 'NONE',  ( -0.2819296736111110979, 4.366750000075866112, 0.000000000000000000 ) ) ;
#11378 = CARTESIAN_POINT ( 'NONE',  ( -0.1236067977499789583, 0.05535714266205806616, -0.3804226065180614791 ) ) ;
#11379 = CARTESIAN_POINT ( 'NONE',  ( -0.2819296736111110424, 4.814666666742533074, 0.1167790944451424923 ) ) ;
#11380 = CARTESIAN_POINT ( 'NONE',  ( 0.1167790944451424506, 4.481333333409199149, 0.2819296736111110424 ) ) ;
#11381 = DIRECTION ( 'NONE',  ( 0.000000000000000000, 0.000000000000000000, -1.000000000000000000 ) ) ;
#11382 = FACE_OUTER_BOUND ( 'NONE', #20129, .T. ) ;
#11383 = CARTESIAN_POINT ( 'NONE',  ( -0.3119999999999998885, 4.061194444596176290, 0.1292346314604058410 ) ) ;
#11384 = DIRECTION ( 'NONE',  ( -0.000000000000000000, -1.000000000000000000, -0.000000000000000000 ) ) ;
#11385 = ADVANCED_FACE ( 'NONE', ( #17486 ), #9367, .T. ) ;
#11386 = CARTESIAN_POINT ( 'NONE',  ( 0.03811151966992424450, -0.3039168590976173978, -0.09500335358987550827 ) ) ;
#11387 = ORIENTED_EDGE ( 'NONE', *, *, #3258, .F. ) ;
#11388 = PERSON_AND_ORGANIZATION_ROLE ( 'creator' ) ;
#11389 = VECTOR ( 'NONE', #3989, 39.37007874015748143 ) ;
#11390 = EDGE_CURVE ( 'NONE', #6124, #1426, #12149, .T. ) ;
#11391 = LINE ( 'NONE', #5775, #23549 ) ;
#11392 = CARTESIAN_POINT ( 'NONE',  ( 3.820898013339742174E-17, 5.384999999999999787, 0.3119999999999999996 ) ) ;
#11393 = ORIENTED_EDGE ( 'NONE', *, *, #17932, .F. ) ;
#11394 = CARTESIAN_POINT ( 'NONE',  ( -0.2206173157302027954, 0.4763888887371559577, -0.2206173157302028232 ) ) ;
#11395 = ORIENTED_EDGE ( 'NONE', *, *, #18397, .T. ) ;
#11396 = LINE ( 'NONE', #18828, #15633 ) ;
#11397 = CARTESIAN_POINT ( 'NONE',  ( 0.04549985820533886810, 0.5149965219823321450, 0.3899922761137797900 ) ) ;
#11398 = CARTESIAN_POINT ( 'NONE',  ( -0.2206173157302027954, 0.5388888888888885287, -0.2206173157302028232 ) ) ;
#11399 = CARTESIAN_POINT ( 'NONE',  ( -0.2923287055106771337, 0.02232142847388617762, -0.2123892367102620804 ) ) ;
#11400 = CARTESIAN_POINT ( 'NONE',  ( 0.2727859317332818612, 3.978974379482379309, -0.1568535693789047114 ) ) ;
#11401 = VERTEX_POINT ( 'NONE', #17138 ) ;
#11402 = CARTESIAN_POINT ( 'NONE',  ( 0.3613381517857143232, 0.1544642856167432743, 0.000000000000000000 ) ) ;
#11403 = ORIENTED_EDGE ( 'NONE', *, *, #17380, .F. ) ;
#11404 = CARTESIAN_POINT ( 'NONE',  ( 0.4872114317030045716, 2.978485840173427324, -1.400868860739402422 ) ) ;
#11405 = CARTESIAN_POINT ( 'NONE',  ( -0.1909016353860534532, 4.676933550353267854, 0.2504354235555140140 ) ) ;
#11406 = CARTESIAN_POINT ( 'NONE',  ( -1.726321361862525858E-17, 3.950083333409199149, -0.2819296736111110979 ) ) ;
#11407 = CARTESIAN_POINT ( 'NONE',  ( -0.3112631253509005602, -0.3615580281551280528, 0.4252366019055051072 ) ) ;
#11408 = CARTESIAN_POINT ( 'NONE',  ( -0.3119999999999998885, 4.832027777777777366, 0.1292346314604058410 ) ) ;
#11409 = CARTESIAN_POINT ( 'NONE',  ( -0.1292346314604057023, 3.838972222222221564, 0.3119999999999998885 ) ) ;
#11410 = CARTESIAN_POINT ( 'NONE',  ( -1.910449006669871087E-17, 4.710500000151732536, -0.3119999999999999996 ) ) ;
#11411 = AXIS2_PLACEMENT_3D ( 'NONE', #20522, #4173, #17230 ) ;
#11412 = CARTESIAN_POINT ( 'NONE',  ( -0.1167790944451423535, 4.932722222298088433, 0.2819296736111110979 ) ) ;
#11413 = EDGE_CURVE ( 'NONE', #22186, #16785, #14436, .T. ) ;
#11414 = EDGE_CURVE ( 'NONE', #3381, #23182, #4953, .T. ) ;
#11415 = CARTESIAN_POINT ( 'NONE',  ( 0.1993543840281266633, 4.332027777853642903, -0.1993543840281266910 ) ) ;
#11416 = EDGE_CURVE ( 'NONE', #404, #12951, #22609, .T. ) ;
#11417 = CARTESIAN_POINT ( 'NONE',  ( -0.2025283230813139379, 3.898705486534137066, 0.2391110646586180055 ) ) ;
#11418 = ORIENTED_EDGE ( 'NONE', *, *, #21712, .T. ) ;
#11419 = CARTESIAN_POINT ( 'NONE',  ( 0.3613381517857143232, 0.2116071427596004084, -0.1174058825155740587 ) ) ;
#11420 = ORIENTED_EDGE ( 'NONE', *, *, #677, .T. ) ;
#11421 = EDGE_LOOP ( 'NONE', ( #13935, #10967, #14584, #9653 ) ) ;
#11422 = MECHANICAL_CONTEXT ( 'NONE', #20566, 'mechanical' ) ;
#11423 = EDGE_CURVE ( 'NONE', #19937, #20410, #900, .T. ) ;
#11424 = CARTESIAN_POINT ( 'NONE',  ( 0.000000000000000000, 5.072999999999999510, 0.000000000000000000 ) ) ;
#11425 = CARTESIAN_POINT ( 'NONE',  ( -0.1167790944451423535, 5.029944444520310753, 0.2819296736111110424 ) ) ;
#11426 = CARTESIAN_POINT ( 'NONE',  ( -0.2819296736111110979, 3.807722222298088877, -0.1167790944451422980 ) ) ;
#11427 = VECTOR ( 'NONE', #2035, 39.37007874015748143 ) ;
#11428 = CARTESIAN_POINT ( 'NONE',  ( 1.020000000000000018, 2.740039370078740433, -2.591000000000000192 ) ) ;
#11429 = CARTESIAN_POINT ( 'NONE',  ( 0.3838280543219422247, 0.3196626468799559362, 0.06591465713332961274 ) ) ;
#11430 = CARTESIAN_POINT ( 'NONE',  ( 0.1583113556674259903, -0.4498647735549116122, 0.08855526556984566477 ) ) ;
#11431 = CARTESIAN_POINT ( 'NONE',  ( 0.1144950937579609085, -0.2764156081756484751, 0.3279166666666704644 ) ) ;
#11432 = CARTESIAN_POINT ( 'NONE',  ( -5.178964085587577574E-17, 0.4798611110352444253, 0.2819296736111110979 ) ) ;
#11433 = CARTESIAN_POINT ( 'NONE',  ( -0.1144950937579609779, 0.2764156081756484196, 0.4181944444444490316 ) ) ;
#11434 = CARTESIAN_POINT ( 'NONE',  ( -0.1167790944451423257, 4.856333333409199149, -0.2819296736111110424 ) ) ;
#11435 = CARTESIAN_POINT ( 'NONE',  ( 0.2922484174926198719, 4.471234547107716395, 0.1097235258941094554 ) ) ;
#11436 = CARTESIAN_POINT ( 'NONE',  ( 0.2819296736111110979, 4.932722222298088433, 0.1167790944451422425 ) ) ;
#11437 = CARTESIAN_POINT ( 'NONE',  ( -0.4593750000000003664, -6.734002413227273428E-17, 0.4343810118395207698 ) ) ;
#11438 = EDGE_CURVE ( 'NONE', #2426, #8700, #9334, .T. ) ;
#11439 = CARTESIAN_POINT ( 'NONE',  ( 0.1976131576089550368, 4.855479579813982483, 0.2418934624741892470 ) ) ;
#11440 = CARTESIAN_POINT ( 'NONE',  ( -0.1085914856217282259, -6.721771644361021011E-18, 0.3623080614478384476 ) ) ;
#11441 = DIRECTION ( 'NONE',  ( 0.5773502691896256200, -0.5773502691896257311, -0.5773502691896256200 ) ) ;
#11442 = CARTESIAN_POINT ( 'NONE',  ( 0.3119999999999999996, 4.408416666666666650, 0.1292346314604056190 ) ) ;
#11443 = CARTESIAN_POINT ( 'NONE',  ( -0.1167790944451423535, 3.863277777853643347, 0.2819296736111110979 ) ) ;
#11444 = DIRECTION ( 'NONE',  ( 0.4472135954999560403, -0.4472135954999560403, 0.7745966692414856247 ) ) ;
#11445 = CARTESIAN_POINT ( 'NONE',  ( -0.3119999999999999996, 0.5388888887371559022, -3.820898013339742174E-17 ) ) ;
#11446 = ORIENTED_EDGE ( 'NONE', *, *, #4410, .F. ) ;
#11447 = CARTESIAN_POINT ( 'NONE',  ( 1.910449006669871087E-17, 0.08055555540382261515, -0.3119999999999999996 ) ) ;
#11448 = ORIENTED_EDGE ( 'NONE', *, *, #14975, .T. ) ;
#11449 = AXIS2_PLACEMENT_3D ( 'NONE', #5603, #22428, #11101 ) ;
#11450 = CARTESIAN_POINT ( 'NONE',  ( -0.2730703793714975292, -0.3836086203274272077, 0.4181140142936807802 ) ) ;
#11451 = ADVANCED_FACE ( 'NONE', ( #21504 ), #20528, .F. ) ;
#11452 = CARTESIAN_POINT ( 'NONE',  ( 0.000000000000000000, -3.937007874019685528E-05, 0.000000000000000000 ) ) ;
#11453 = CARTESIAN_POINT ( 'NONE',  ( -0.3155070326520293400, 0.1306872919485614903, -0.1599305555555554370 ) ) ;
#11454 = B_SPLINE_CURVE_WITH_KNOTS ( 'NONE', 3,
 ( #18319, #18558, #21855, #21973, #10891, #21740, #5265, #12735, #20151, #3440, #1617, #9051, #16497, #9171, #23909, #16616, #7345, #14797, #22212, #3683, #8685, #16133, #5025, #20867, #22330, #17215, #2345, #16967 ),
 .UNSPECIFIED., .F., .F.,
 ( 4, 2, 2, 2, 2, 2, 2, 2, 2, 2, 2, 2, 2, 4 ),
 ( 0.1142854809683468142, 0.1163847642462578491, 0.1184840475241688840, 0.1195336891631243875, 0.1205833308020799050, 0.1216329724410354224, 0.1226826140799909398, 0.1237322557189464572, 0.1247818973579019747, 0.1258315389968574782, 0.1268811806358129957, 0.1279308222747685131, 0.1289804639137240305, 0.1310797471916350654 ),
 .UNSPECIFIED. ) ;
#11455 = CARTESIAN_POINT ( 'NONE',  ( 0.3949999999999999623, 2.978485840173427324, -0.04999999999999919092 ) ) ;
#11456 = CARTESIAN_POINT ( 'NONE',  ( 0.2414151976196820815, 5.152793932359630347, -0.1819029909458831917 ) ) ;
#11457 = EDGE_LOOP ( 'NONE', ( #21489, #7787, #6148, #12756 ) ) ;
#11458 = CARTESIAN_POINT ( 'NONE',  ( -0.3613381517857144343, 0.03303571418817188854, 0.1174058825155740171 ) ) ;
#11459 = CARTESIAN_POINT ( 'NONE',  ( -0.1993543840281267465, 0.5701388888130222155, 0.1993543840281266633 ) ) ;
#11460 = CARTESIAN_POINT ( 'NONE',  ( 0.1144950937579609085, -0.2764156081756484751, -0.1095833333333330467 ) ) ;
#11461 = CARTESIAN_POINT ( 'NONE',  ( 0.2947906553666733709, 0.5822185911807998826, -1.096288212844231724 ) ) ;
#11462 = DIRECTION ( 'NONE',  ( 0.4254442446013927959, -0.6399207742898898044, -0.6399207742898944673 ) ) ;
#11463 = CARTESIAN_POINT ( 'NONE',  ( -0.1954553509668046640, 0.1954553509668046918, 0.2550000000000031686 ) ) ;
#11464 = AXIS2_PLACEMENT_3D ( 'NONE', #23466, #14469, #8355 ) ;
#11465 = VERTEX_POINT ( 'NONE', #15897 ) ;
#11466 = CARTESIAN_POINT ( 'NONE',  ( -0.2945206866155428704, 5.108041754680044733, 0.09890754808314189406 ) ) ;
#11467 = CARTESIAN_POINT ( 'NONE',  ( 0.2998642343065497373, 0.08796414601275419354, 0.4241666666666771834 ) ) ;
#11468 = CARTESIAN_POINT ( 'NONE',  ( 0.3119999999999998885, 0.3479166666666663188, 0.1292346314604058410 ) ) ;
#11469 = CARTESIAN_POINT ( 'NONE',  ( 0.1292346314604058410, 5.234805555555554157, 0.3119999999999998885 ) ) ;
#11470 = CARTESIAN_POINT ( 'NONE',  ( 5.178964085587577574E-17, 4.213972222298087544, 0.2819296736111110979 ) ) ;
#11471 = LINE ( 'NONE', #7913, #1480 ) ;
#11472 = DIRECTION ( 'NONE',  ( -1.000000000000000000, 0.000000000000000000, 0.000000000000000000 ) ) ;
#11473 = ORIENTED_EDGE ( 'NONE', *, *, #1309, .T. ) ;
#11474 = CARTESIAN_POINT ( 'NONE',  ( 0.2206173157302027676, 0.3444444444444440534, 0.2206173157302028787 ) ) ;
#11475 = CARTESIAN_POINT ( 'NONE',  ( 0.1993543840281266633, 4.887583333409199149, -0.1993543840281266910 ) ) ;
#11476 = CARTESIAN_POINT ( 'NONE',  ( 0.01740894572980225888, 5.198436972620729790, 0.2852777632786984152 ) ) ;
#11477 = CARTESIAN_POINT ( 'NONE',  ( -0.2195237376300352150, 5.149645692627588645, -0.2082703641299125108 ) ) ;
#11478 = AXIS2_PLACEMENT_3D ( 'NONE', #9835, #15441, #16902 ) ;
#11479 = DIRECTION ( 'NONE',  ( -0.000000000000000000, -1.000000000000000000, -0.000000000000000000 ) ) ;
#11480 = DIRECTION ( 'NONE',  ( 4.347502568299317526E-16, 0.7071067811865511255, 0.7071067811865439090 ) ) ;
#11481 = CARTESIAN_POINT ( 'NONE',  ( 0.2819296736111110979, 4.342444444520310753, -0.1167790944451423396 ) ) ;
#11482 = CALENDAR_DATE ( 2026, 7, 10 ) ;
#11483 = VERTEX_POINT ( 'NONE', #14562 ) ;
#11484 = CARTESIAN_POINT ( 'NONE',  ( -0.01981372967188622242, 4.044372679049708985, -0.3113707790481334281 ) ) ;
#11485 =( BOUNDED_SURFACE ( )  B_SPLINE_SURFACE ( 1, 2, ( 
 ( #4668, #3315, #18076, #10295, #8443, #16132, #17964, #3198, #14304, #10773, #1376, #23787, #8930, #21614, #4908, #8805, #3087, #6861, #18199, #7107, #14547, #17717, #12137, #21738, #16254, #8683, #6984, #14427, #19544, #21853, #5142, #2835, #12609, #1013, #21493, #4782, #12250, #22454, #11, #260, #16496, #12853, #7459, #10889, #23907, #3557, #1846, #9169, #16614, #1731, #14908, #3804, #12972, #24033, #5388, #22328, #5629, #11368, #16965, #20388, #1614, #20149, #9049, #3681, #5753, #16850, #18795, #7343, #20509, #7227, #11127, #3438, #14795, #18317, #1975, #22210, #13095, #7700, #5510, #16731, #137, #22092, #18556, #14673, #13214, #11007, #21971, #9289, #11250, #20270, #18674, #9413, #7580, #15029, #18436, #20623, #3923, #2090, #9532, #5263, #12733, #2343, #13573, #20982, #9899, #624, #20866, #2460, #4396, #17213, #22930, #21107, #10026, #2578, #7820, #4159, #9781, #6348, #13689, #17330, #10146, #15265, #17570, #13798, #8170, #6103, #5864, #11983, #9654, #497, #2694, #17448, #18924, #8055, #6225, #5983, #4278, #15503, #11858, #19154, #19273, #742, #15624, #11733, #13323, #7931, #860, #15385, #23043, #21229, #4518, #22813, #13447, #19396, #11610, #2223, #15147, #22576, #20745, #4037, #11491, #17093, #19041, #379, #22692, #1100, #19995, #10615, #12103, #3051, #16099, #23274, #23397, #19756, #4990, #12340, #12454, #10498, #19873, #6705, #6466 ),
 ( #23513, #4873, #23636, #17687, #5108, #8291, #6953, #21706, #13920, #19513, #17928, #14149, #6829, #1224, #14394, #14270, #3283, #12574, #8533, #12220, #3165, #19630, #8650, #21818, #10737, #18167, #21348, #15745, #18045, #1341, #2929, #8771, #10387, #23156, #16224, #21578, #4638, #6586, #2806, #10261, #980, #8409, #15857, #14035, #21465, #4749, #17809, #15976, #7076, #9136, #5480, #1815, #14881, #15000, #5724, #23873, #5355, #22298, #12821, #7193, #16581, #20357, #24119, #20240, #3529, #20478, #5595, #5228, #14638, #3892, #12702, #22422, #10980, #22061, #10858, #18287, #13060, #1584, #18406, #7434, #3774, #1699, #7314, #11216, #12945, #24002, #14764, #1938, #18645, #9385, #9259, #16825, #3647, #7548, #22180, #11094, #18525, #13183, #16342, #16700, #107, #20596, #11337, #1463, #8898, #23754, #14514, #9020, #16461, #21935, #20117, #3408, #18766, #11701, #15352, #9993, #2545, #4127, #2428, #22781, #17418, #4011, #15591, #2061, #711, #8022, #234, #22546, #6075, #469, #17297, #4249, #8139, #590, #13767, #23013, #11584, #22664, #9870, #5953, #13541, #6315, #21193, #4484, #7670, #9502, #19124, #15473, #13412, #20956, #20835, #16936, #22899, #9746, #15120, #9624, #7900, #13659, #5837, #13300, #19241, #17183, #6193, #15235, #21074, #19013, #20715, #2309, #4364, #11822, #11459, #18892, #2193, #17057, #350, #7791, #23242, #17655, #19598, #6674, #10469 ) ),
 .UNSPECIFIED., .F., .F., .F. ) 
 B_SPLINE_SURFACE_WITH_KNOTS ( ( 2, 2 ),
 ( 3, 2, 2, 2, 2, 2, 2, 2, 2, 2, 2, 2, 2, 2, 2, 2, 2, 2, 2, 2, 2, 2, 2, 2, 2, 2, 2, 2, 2, 2, 2, 2, 2, 2, 2, 2, 2, 2, 2, 2, 2, 2, 2, 2, 2, 2, 2, 2, 2, 2, 2, 2, 2, 2, 2, 2, 2, 2, 2, 2, 2, 2, 2, 2, 2, 2, 2, 2, 2, 2, 2, 2, 2, 2, 2, 2, 2, 2, 2, 2, 2, 2, 2, 2, 2, 2, 2, 2, 2, 2, 3 ),
 ( 0.000000000000000000, 1.000000000000000000 ),
 ( 0.000000000000000000, 0.01041666666666666609, 0.02083333333333333218, 0.03125000000000000000, 0.04166666666666666435, 0.05208333333333333565, 0.06250000000000000000, 0.07291666666666667129, 0.08333333333333332871, 0.09375000000000000000, 0.1041666666666666713, 0.1145833333333333287, 0.1250000000000000000, 0.1354166666666666574, 0.1458333333333333426, 0.1562500000000000000, 0.1666666666666666574, 0.1770833333333333426, 0.1875000000000000000, 0.1979166666666666574, 0.2083333333333333426, 0.2187500000000000000, 0.2291666666666666574, 0.2395833333333333426, 0.2500000000000000000, 0.2604166666666666852, 0.2708333333333333148, 0.2812500000000000000, 0.2916666666666666852, 0.3020833333333333148, 0.3125000000000000000, 0.3229166666666666852, 0.3333333333333333148, 0.3437500000000000000, 0.3541666666666666852, 0.3645833333333333148, 0.3750000000000000000, 0.3854166666666666852, 0.3958333333333333148, 0.4062500000000000000, 0.4166666666666666852, 0.4270833333333333148, 0.4375000000000000000, 0.4479166666666666852, 0.4583333333333333148, 0.4687500000000000000, 0.4791666666666666852, 0.4895833333333333148, 0.5000000000000000000, 0.5104166666666666297, 0.5208333333333333703, 0.5312500000000000000, 0.5416666666666666297, 0.5520833333333333703, 0.5625000000000000000, 0.5729166666666666297, 0.5833333333333333703, 0.5937500000000000000, 0.6041666666666666297, 0.6145833333333333703, 0.6250000000000000000, 0.6354166666666666297, 0.6458333333333333703, 0.6562500000000000000, 0.6666666666666666297, 0.6770833333333333703, 0.6875000000000000000, 0.6979166666666666297, 0.7083333333333333703, 0.7187500000000000000, 0.7291666666666666297, 0.7395833333333333703, 0.7500000000000000000, 0.7604166666666666297, 0.7708333333333333703, 0.7812500000000000000, 0.7916666666666666297, 0.8020833333333333703, 0.8125000000000000000, 0.8229166666666666297, 0.8333333333333333703, 0.8437500000000000000, 0.8541666666666666297, 0.8645833333333333703, 0.8750000000000000000, 0.8854166666666666297, 0.8958333333333333703, 0.9062500000000000000, 0.9166666666666666297, 0.9270833333333333703, 0.9375000000000000000 ),
 .UNSPECIFIED. ) 
 GEOMETRIC_REPRESENTATION_ITEM ( )  RATIONAL_B_SPLINE_SURFACE ( (
 ( 1.000000000000000000, 0.9238795325112867385, 1.000000000000000000, 0.9238795325112867385, 1.000000000000000000, 0.9238795325112867385, 1.000000000000000000, 0.9238795325112867385, 1.000000000000000000, 0.9238795325112867385, 1.000000000000000000, 0.9238795325112867385, 1.000000000000000000, 0.9238795325112867385, 1.000000000000000000, 0.9238795325112867385, 1.000000000000000000, 0.9238795325112867385, 1.000000000000000000, 0.9238795325112867385, 1.000000000000000000, 0.9238795325112867385, 1.000000000000000000, 0.9238795325112867385, 1.000000000000000000, 0.9238795325112867385, 1.000000000000000000, 0.9238795325112867385, 1.000000000000000000, 0.9238795325112867385, 1.000000000000000000, 0.9238795325112867385, 1.000000000000000000, 0.9238795325112867385, 1.000000000000000000, 0.9238795325112867385, 1.000000000000000000, 0.9238795325112867385, 1.000000000000000000, 0.9238795325112867385, 1.000000000000000000, 0.9238795325112867385, 1.000000000000000000, 0.9238795325112867385, 1.000000000000000000, 0.9238795325112867385, 1.000000000000000000, 0.9238795325112867385, 1.000000000000000000, 0.9238795325112867385, 1.000000000000000000, 0.9238795325112867385, 1.000000000000000000, 0.9238795325112867385, 1.000000000000000000, 0.9238795325112867385, 1.000000000000000000, 0.9238795325112867385, 1.000000000000000000, 0.9238795325112867385, 1.000000000000000000, 0.9238795325112867385, 1.000000000000000000, 0.9238795325112867385, 1.000000000000000000, 0.9238795325112867385, 1.000000000000000000, 0.9238795325112867385, 1.000000000000000000, 0.9238795325112867385, 1.000000000000000000, 0.9238795325112867385, 1.000000000000000000, 0.9238795325112867385, 1.000000000000000000, 0.9238795325112867385, 1.000000000000000000, 0.9238795325112867385, 1.000000000000000000, 0.9238795325112867385, 1.000000000000000000, 0.9238795325112867385, 1.000000000000000000, 0.9238795325112867385, 1.000000000000000000, 0.9238795325112867385, 1.000000000000000000, 0.9238795325112867385, 1.000000000000000000, 0.9238795325112867385, 1.000000000000000000, 0.9238795325112867385, 1.000000000000000000, 0.9238795325112867385, 1.000000000000000000, 0.9238795325112867385, 1.000000000000000000, 0.9238795325112867385, 1.000000000000000000, 0.9238795325112867385, 1.000000000000000000, 0.9238795325112867385, 1.000000000000000000, 0.9238795325112867385, 1.000000000000000000, 0.9238795325112867385, 1.000000000000000000, 0.9238795325112867385, 1.000000000000000000, 0.9238795325112867385, 1.000000000000000000, 0.9238795325112867385, 1.000000000000000000, 0.9238795325112867385, 1.000000000000000000, 0.9238795325112867385, 1.000000000000000000, 0.9238795325112867385, 1.000000000000000000, 0.9238795325112867385, 1.000000000000000000, 0.9238795325112867385, 1.000000000000000000, 0.9238795325112867385, 1.000000000000000000, 0.9238795325112867385, 1.000000000000000000, 0.9238795325112867385, 1.000000000000000000, 0.9238795325112867385, 1.000000000000000000, 0.9238795325112867385, 1.000000000000000000, 0.9238795325112867385, 1.000000000000000000, 0.9238795325112867385, 1.000000000000000000, 0.9238795325112867385, 1.000000000000000000, 0.9238795325112867385, 1.000000000000000000, 0.9238795325112867385, 1.000000000000000000, 0.9238795325112867385, 1.000000000000000000, 0.9238795325112867385, 1.000000000000000000, 0.9238795325112867385, 1.000000000000000000, 0.9238795325112867385, 1.000000000000000000, 0.9238795325112867385, 1.000000000000000000, 0.9238795325112867385, 1.000000000000000000, 0.9238795325112867385, 1.000000000000000000, 0.9238795325112867385, 1.000000000000000000, 0.9238795325112867385, 1.000000000000000000, 0.9238795325112867385, 1.000000000000000000, 0.9238795325112867385, 1.000000000000000000, 0.9238795325112867385, 1.000000000000000000, 0.9238795325112867385, 1.000000000000000000, 0.9238795325112867385, 1.000000000000000000, 0.9238795325112867385, 1.000000000000000000, 0.9238795325112867385, 1.000000000000000000, 0.9238795325112867385, 1.000000000000000000, 0.9238795325112867385, 1.000000000000000000, 0.9238795325112867385, 1.000000000000000000),
 ( 1.000000000000000000, 0.9238795325112867385, 1.000000000000000000, 0.9238795325112867385, 1.000000000000000000, 0.9238795325112867385, 1.000000000000000000, 0.9238795325112867385, 1.000000000000000000, 0.9238795325112867385, 1.000000000000000000, 0.9238795325112867385, 1.000000000000000000, 0.9238795325112867385, 1.000000000000000000, 0.9238795325112867385, 1.000000000000000000, 0.9238795325112867385, 1.000000000000000000, 0.9238795325112867385, 1.000000000000000000, 0.9238795325112867385, 1.000000000000000000, 0.9238795325112867385, 1.000000000000000000, 0.9238795325112867385, 1.000000000000000000, 0.9238795325112867385, 1.000000000000000000, 0.9238795325112867385, 1.000000000000000000, 0.9238795325112867385, 1.000000000000000000, 0.9238795325112867385, 1.000000000000000000, 0.9238795325112867385, 1.000000000000000000, 0.9238795325112867385, 1.000000000000000000, 0.9238795325112867385, 1.000000000000000000, 0.9238795325112867385, 1.000000000000000000, 0.9238795325112867385, 1.000000000000000000, 0.9238795325112867385, 1.000000000000000000, 0.9238795325112867385, 1.000000000000000000, 0.9238795325112867385, 1.000000000000000000, 0.9238795325112867385, 1.000000000000000000, 0.9238795325112867385, 1.000000000000000000, 0.9238795325112867385, 1.000000000000000000, 0.9238795325112867385, 1.000000000000000000, 0.9238795325112867385, 1.000000000000000000, 0.9238795325112867385, 1.000000000000000000, 0.9238795325112867385, 1.000000000000000000, 0.9238795325112867385, 1.000000000000000000, 0.9238795325112867385, 1.000000000000000000, 0.9238795325112867385, 1.000000000000000000, 0.9238795325112867385, 1.000000000000000000, 0.9238795325112867385, 1.000000000000000000, 0.9238795325112867385, 1.000000000000000000, 0.9238795325112867385, 1.000000000000000000, 0.9238795325112867385, 1.000000000000000000, 0.9238795325112867385, 1.000000000000000000, 0.9238795325112867385, 1.000000000000000000, 0.9238795325112867385, 1.000000000000000000, 0.9238795325112867385, 1.000000000000000000, 0.9238795325112867385, 1.000000000000000000, 0.9238795325112867385, 1.000000000000000000, 0.9238795325112867385, 1.000000000000000000, 0.9238795325112867385, 1.000000000000000000, 0.9238795325112867385, 1.000000000000000000, 0.9238795325112867385, 1.000000000000000000, 0.9238795325112867385, 1.000000000000000000, 0.9238795325112867385, 1.000000000000000000, 0.9238795325112867385, 1.000000000000000000, 0.9238795325112867385, 1.000000000000000000, 0.9238795325112867385, 1.000000000000000000, 0.9238795325112867385, 1.000000000000000000, 0.9238795325112867385, 1.000000000000000000, 0.9238795325112867385, 1.000000000000000000, 0.9238795325112867385, 1.000000000000000000, 0.9238795325112867385, 1.000000000000000000, 0.9238795325112867385, 1.000000000000000000, 0.9238795325112867385, 1.000000000000000000, 0.9238795325112867385, 1.000000000000000000, 0.9238795325112867385, 1.000000000000000000, 0.9238795325112867385, 1.000000000000000000, 0.9238795325112867385, 1.000000000000000000, 0.9238795325112867385, 1.000000000000000000, 0.9238795325112867385, 1.000000000000000000, 0.9238795325112867385, 1.000000000000000000, 0.9238795325112867385, 1.000000000000000000, 0.9238795325112867385, 1.000000000000000000, 0.9238795325112867385, 1.000000000000000000, 0.9238795325112867385, 1.000000000000000000, 0.9238795325112867385, 1.000000000000000000, 0.9238795325112867385, 1.000000000000000000, 0.9238795325112867385, 1.000000000000000000, 0.9238795325112867385, 1.000000000000000000, 0.9238795325112867385, 1.000000000000000000, 0.9238795325112867385, 1.000000000000000000, 0.9238795325112867385, 1.000000000000000000, 0.9238795325112867385, 1.000000000000000000, 0.9238795325112867385, 1.000000000000000000, 0.9238795325112867385, 1.000000000000000000, 0.9238795325112867385, 1.000000000000000000, 0.9238795325112867385, 1.000000000000000000, 0.9238795325112867385, 1.000000000000000000, 0.9238795325112867385, 1.000000000000000000, 0.9238795325112867385, 1.000000000000000000, 0.9238795325112867385, 1.000000000000000000, 0.9238795325112867385, 1.000000000000000000) ) ) 
 REPRESENTATION_ITEM ( '' )  SURFACE ( )  );
#11486 = CARTESIAN_POINT ( 'NONE',  ( 0.1144950937579609085, -0.2764156081756484751, 0.001527777777778949230 ) ) ;
#11487 =( BOUNDED_CURVE ( )  B_SPLINE_CURVE ( 2, ( #17505, #15680, #19454, #21288, #2401, #6161, #11786, #8347, #8228 ),
 .UNSPECIFIED., .F., .T. ) 
 B_SPLINE_CURVE_WITH_KNOTS ( ( 3, 2, 2, 2, 3 ),
 ( 0.7812500000000001110, 0.7916666666666668517, 0.8020833333333334814, 0.8125000000000000000, 0.8229166666666667407 ),
 .UNSPECIFIED. ) 
 CURVE ( )  GEOMETRIC_REPRESENTATION_ITEM ( )  RATIONAL_B_SPLINE_CURVE ( ( 0.9999999999999992228, 0.9238795325112875156, 1.000000000000000000, 0.9238795325112867385, 1.000000000000000000, 0.9238795325112867385, 1.000000000000000000, 0.9238795325112867385, 1.000000000000000000 ) ) 
 REPRESENTATION_ITEM ( '' )  );
#11488 = AXIS2_PLACEMENT_3D ( 'NONE', #2362, #11631, #13591 ) ;
#11489 = CARTESIAN_POINT ( 'NONE',  ( 1.726321361862525858E-17, 0.4520833332574667462, -0.2819296736111110979 ) ) ;
#11490 = ORIENTED_EDGE ( 'NONE', *, *, #3639, .F. ) ;
#11491 = CARTESIAN_POINT ( 'NONE',  ( 0.2819296736111110979, 0.5493055554796889561, 0.000000000000000000 ) ) ;
#11492 = CYLINDRICAL_SURFACE ( 'NONE', #16631, 0.3125000000000000000 ) ;
#11493 = CARTESIAN_POINT ( 'NONE',  ( -0.4000000000000000222, 0.2214285714285713358, -4.898587196589413075E-17 ) ) ;
#11494 = CARTESIAN_POINT ( 'NONE',  ( 0.000000000000000000, 0.3155070326520292845, 0.1595138888888911199 ) ) ;
#11495 = CARTESIAN_POINT ( 'NONE',  ( -0.3838280543219043661, -0.3196626468799559362, 0.06591465713332006482 ) ) ;
#11496 = LINE ( 'NONE', #11615, #18690 ) ;
#11497 = CARTESIAN_POINT ( 'NONE',  ( 0.1993543840281266910, 0.2090277777019111383, -0.1993543840281266910 ) ) ;
#11498 = CARTESIAN_POINT ( 'NONE',  ( 0.1167790944451423257, 0.3236111110352444808, -0.2819296736111110424 ) ) ;
#11499 = ORIENTED_EDGE ( 'NONE', *, *, #3310, .F. ) ;
#11500 = CARTESIAN_POINT ( 'NONE',  ( 0.2819296736111110979, 4.335500000075866112, 0.1167790944451422425 ) ) ;
#11501 = CARTESIAN_POINT ( 'NONE',  ( 0.1236067977499789861, 0.4053571426620580787, -0.3804226065180614236 ) ) ;
#11502 = AXIS2_PLACEMENT_3D ( 'NONE', #12183, #10341, #1305 ) ;
#11503 = CARTESIAN_POINT ( 'NONE',  ( -0.2819296736111110424, 4.925777777853643791, 0.1167790944451424923 ) ) ;
#11504 = CARTESIAN_POINT ( 'NONE',  ( 0.2819296736111111534, 4.543833333409198261, 0.1167790944451422563 ) ) ;
#11505 = CARTESIAN_POINT ( 'NONE',  ( 0.000000000000000000, 0.8699999999999998845, 0.000000000000000000 ) ) ;
#11506 = CARTESIAN_POINT ( 'NONE',  ( 0.2935666255429962290, 2.563566625542996302, -0.5657204318808580767 ) ) ;
#11507 = CARTESIAN_POINT ( 'NONE',  ( 0.3119999999999999996, 4.029944444596176290, -3.820898013339742174E-17 ) ) ;
#11508 = LOCAL_TIME ( 21, 9, 13.00000000000000000, #4740 ) ;
#11509 = CARTESIAN_POINT ( 'NONE',  ( -0.06335377612981497875, 0.2679019384315882712, -0.3999999999999999667 ) ) ;
#11510 = CARTESIAN_POINT ( 'NONE',  ( 0.2256529556067323194, -0.2011140187169014881, -0.09097104604570598052 ) ) ;
#11511 = ORIENTED_EDGE ( 'NONE', *, *, #12472, .F. ) ;
#11512 = APPROVAL_DATE_TIME ( #22947, #5523 ) ;
#11513 = AXIS2_PLACEMENT_3D ( 'NONE', #1281, #8706, #14328 ) ;
#11514 = CARTESIAN_POINT ( 'NONE',  ( 0.4872114317030045716, 2.291712385858714729, -1.340783969076326132 ) ) ;
#11515 = DIRECTION ( 'NONE',  ( 0.000000000000000000, 0.000000000000000000, -1.000000000000000000 ) ) ;
#11516 = CARTESIAN_POINT ( 'NONE',  ( 0.7108475124358174524, 3.066692553488282957, 2.927961747820534644 ) ) ;
#11517 = ORIENTED_EDGE ( 'NONE', *, *, #18095, .F. ) ;
#11518 = CARTESIAN_POINT ( 'NONE',  ( -5.731347020009612645E-17, 0.6083333331816004330, 0.3119999999999999996 ) ) ;
#11519 = ORIENTED_EDGE ( 'NONE', *, *, #18421, .T. ) ;
#11520 = CARTESIAN_POINT ( 'NONE',  ( 0.1670718646175240740, 4.261161593087173571, -0.2643034011721546173 ) ) ;
#11521 = CYLINDRICAL_SURFACE ( 'NONE', #1091, 0.3119999999999999996 ) ;
#11522 = CARTESIAN_POINT ( 'NONE',  ( 0.3037029041911168403, 4.749794205331636654, 0.08231968813497411719 ) ) ;
#11523 = CARTESIAN_POINT ( 'NONE',  ( 0.2923287055106771337, 0.0008928570453147542749, -0.2123892367102620249 ) ) ;
#11524 = CARTESIAN_POINT ( 'NONE',  ( 0.1300715219937130795, 5.170735578853760117, 0.2669230633663410290 ) ) ;
#11525 = ORIENTED_EDGE ( 'NONE', *, *, #18697, .F. ) ;
#11526 = PRODUCT_DEFINITION_FORMATION_WITH_SPECIFIED_SOURCE ( 'ANY', '', #18099, .NOT_KNOWN. ) ;
#11527 = CARTESIAN_POINT ( 'NONE',  ( 0.2923287055106771337, 0.3044642856167432687, -0.2123892367102620249 ) ) ;
#11528 = CARTESIAN_POINT ( 'NONE',  ( 0.7919466436700954848, 2.665000000000000036, -2.986000000000000210 ) ) ;
#11529 = CARTESIAN_POINT ( 'NONE',  ( -0.1954553509668046640, 0.1954553509668046918, 0.4147222222222267107 ) ) ;
#11530 = EDGE_CURVE ( 'NONE', #9562, #23454, #3796, .T. ) ;
#11531 = CARTESIAN_POINT ( 'NONE',  ( -0.2819296736111110424, 3.967444444520310309, 0.1167790944451424923 ) ) ;
#11532 = DIRECTION ( 'NONE',  ( 0.000000000000000000, 1.000000000000000000, 0.000000000000000000 ) ) ;
#11533 = CARTESIAN_POINT ( 'NONE',  ( 0.4593750000000003664, -0.2760455974562899817, 0.06112444011295372487 ) ) ;
#11534 = CARTESIAN_POINT ( 'NONE',  ( 0.6082799348109491078, 3.738202056031992182, 0.09828638484944851594 ) ) ;
#11535 = CLOSED_SHELL ( 'NONE', ( #2329, #23180, #19884, #23316, #7030, #3704, #19612, #433, #11246, #8235, #3444, #10953, #19859, #5017, #16304, #8630, #18907, #22563, #1525, #20020, #1716, #4927, #20050, #15328, #12606, #23916, #5222, #23451, #14573, #1392, #7497, #11109, #23962, #13230, #17660, #14079, #13089, #8326, #17068, #23010, #62, #1961, #2332, #18063, #13559, #17085, #12066, #19201, #9011, #22741, #19597, #8705, #10666, #3368, #10649, #7224, #12156, #15604, #824, #19596, #30, #4254, #6004, #2963, #12607, #15035, #8865, #5499, #16028, #13789, #5548, #21429, #15138, #17026, #8569, #22113, #21340, #5615, #14235, #1311, #3196, #13625, #17986, #16595, #11351, #7521, #20132 ) ) ;
#11536 = CARTESIAN_POINT ( 'NONE',  ( -0.2206173157302028232, 4.773000000151731648, -0.2206173157302028232 ) ) ;
#11537 = EDGE_CURVE ( 'NONE', #6959, #9037, #18340, .T. ) ;
#11538 = CARTESIAN_POINT ( 'NONE',  ( 0.1993543840281267465, 4.998694444520309865, 0.1993543840281266633 ) ) ;
#11539 = VERTEX_POINT ( 'NONE', #6750 ) ;
#11540 = CARTESIAN_POINT ( 'NONE',  ( 0.2819296736111110424, 4.384111111186976828, -0.1167790944451423396 ) ) ;
#11541 = ORIENTED_EDGE ( 'NONE', *, *, #10374, .F. ) ;
#11542 = CARTESIAN_POINT ( 'NONE',  ( -0.3613381517857143788, 0.1758928570453147100, 0.1174058825155740310 ) ) ;
#11543 = ORIENTED_EDGE ( 'NONE', *, *, #9970, .T. ) ;
#11544 = LOCAL_TIME ( 21, 9, 13.00000000000000000, #16248 ) ;
#11545 = ORIENTED_EDGE ( 'NONE', *, *, #1288, .F. ) ;
#11546 = COORDINATED_UNIVERSAL_TIME_OFFSET ( 0, 0, .AHEAD. ) ;
#11547 = CARTESIAN_POINT ( 'NONE',  ( 0.000000000000000000, 0.000000000000000000, 1.326383476483184332 ) ) ;
#11548 = CYLINDRICAL_SURFACE ( 'NONE', #5385, 0.3119999999999999996 ) ;
#11549 = CARTESIAN_POINT ( 'NONE',  ( 0.1993543840281266633, 3.901472222298087988, -0.1993543840281266910 ) ) ;
#11550 = AXIS2_PLACEMENT_3D ( 'NONE', #3088, #14428, #1136 ) ;
#11551 = CARTESIAN_POINT ( 'NONE',  ( -0.3394572874457115752, 3.700000000000000622, -0.09499999999999993172 ) ) ;
#11552 = CARTESIAN_POINT ( 'NONE',  ( 0.2764156081756483641, -0.1144950937579611028, 0.3418055555555594149 ) ) ;
#11553 = EDGE_CURVE ( 'NONE', #10865, #7634, #3212, .T. ) ;
#11554 = CARTESIAN_POINT ( 'NONE',  ( -1.133296993574655964, 3.066692553488282957, 2.163426826761001287 ) ) ;
#11555 = EDGE_CURVE ( 'NONE', #2739, #23062, #17729, .T. ) ;
#11556 = ORIENTED_EDGE ( 'NONE', *, *, #23749, .F. ) ;
#11557 = CARTESIAN_POINT ( 'NONE',  ( -0.2764156081756484196, 1.692557448933383907E-17, 0.1438888888888912032 ) ) ;
#11558 = CARTESIAN_POINT ( 'NONE',  ( 0.2819296736111110979, 0.4972222221463556413, -0.1167790944451422980 ) ) ;
#11559 = CARTESIAN_POINT ( 'NONE',  ( 0.2764156081756483641, 0.1144950937579610056, 0.4043055555555599145 ) ) ;
#11560 = VERTEX_POINT ( 'NONE', #23319 ) ;
#11561 = CARTESIAN_POINT ( 'NONE',  ( 0.1167790944451424368, 4.995222222298087544, 0.2819296736111110424 ) ) ;
#11562 = CARTESIAN_POINT ( 'NONE',  ( 5.731347020009612645E-17, 3.953555555555555046, 0.3119999999999999996 ) ) ;
#11563 = CARTESIAN_POINT ( 'NONE',  ( 0.2819296736111110979, 4.769527777853642903, -3.452642723725051716E-17 ) ) ;
#11564 = CARTESIAN_POINT ( 'NONE',  ( -0.2107751267066935164, 0.1916353986792941333, -0.07341118351979945833 ) ) ;
#11565 = CARTESIAN_POINT ( 'NONE',  ( 0.1679725729491048092, 4.872240167009049827, -0.2637599262370826092 ) ) ;
#11566 = LOCAL_TIME ( 21, 9, 13.00000000000000000, #4154 ) ;
#11567 = DIRECTION ( 'NONE',  ( 0.000000000000000000, -0.7071067811865514585, 0.7071067811865436870 ) ) ;
#11568 = CARTESIAN_POINT ( 'NONE',  ( 0.4687500000000002776, 0.2598076211353318454, 0.06112444011295372487 ) ) ;
#11569 = CARTESIAN_POINT ( 'NONE',  ( 0.3119999999999999996, 4.522999999999999687, -3.820898013339742174E-17 ) ) ;
#11570 = CARTESIAN_POINT ( 'NONE',  ( -0.1993543840281266355, 3.748694444520309865, 0.1993543840281267465 ) ) ;
#11571 = DIRECTION ( 'NONE',  ( -1.177540334020096140E-17, 0.2588190451025212946, -0.9659258262890679791 ) ) ;
#11572 = EDGE_CURVE ( 'NONE', #13477, #20558, #20165, .T. ) ;
#11573 = CARTESIAN_POINT ( 'NONE',  ( -0.2206173157302027954, 0.5319444442927114824, -0.2206173157302028232 ) ) ;
#11574 = ORIENTED_EDGE ( 'NONE', *, *, #8448, .F. ) ;
#11575 = AXIS2_PLACEMENT_3D ( 'NONE', #13062, #23756, #20480 ) ;
#11576 = DIRECTION ( 'NONE',  ( 0.000000000000000000, 0.000000000000000000, -1.000000000000000000 ) ) ;
#11577 = EDGE_LOOP ( 'NONE', ( #6570, #9867, #21757 ) ) ;
#11578 = CARTESIAN_POINT ( 'NONE',  ( 0.2824805458792227220, 4.700498842312279990, -0.1324723342704639539 ) ) ;
#11579 = CARTESIAN_POINT ( 'NONE',  ( 0.2764156081756483641, -0.1144950937579611167, 0.4459722222222269328 ) ) ;
#11580 = DIRECTION ( 'NONE',  ( 0.4999999999999941158, 0.000000000000000000, -0.8660254037844420383 ) ) ;
#11581 = ORIENTED_EDGE ( 'NONE', *, *, #10414, .T. ) ;
#11582 = CARTESIAN_POINT ( 'NONE',  ( -0.2233192592356399442, 0.01874999990245759460, -0.3073725909049500049 ) ) ;
#11583 = TOROIDAL_SURFACE ( 'NONE', #1059, 1.015181661097394050, 0.03500000000000000333 ) ;
#11584 = CARTESIAN_POINT ( 'NONE',  ( -0.2819296736111110979, 0.4520833332574666907, -3.452642723725051716E-17 ) ) ;
#11585 = CARTESIAN_POINT ( 'NONE',  ( -0.1950097289954165203, 5.206640035683668621, 0.2045561157895784965 ) ) ;
#11586 = CARTESIAN_POINT ( 'NONE',  ( -1.515315767888941311E-17, 0.1799999999999999933, -1.242999999999999661 ) ) ;
#11587 = CARTESIAN_POINT ( 'NONE',  ( -0.1292346314604058410, 0.1673611111111107941, 0.3119999999999998885 ) ) ;
#11588 = CARTESIAN_POINT ( 'NONE',  ( 0.000000000000000000, 0.2764156081756484196, 0.1369444444444467002 ) ) ;
#11589 = DIRECTION ( 'NONE',  ( 0.000000000000000000, 0.000000000000000000, -1.000000000000000000 ) ) ;
#11590 = CARTESIAN_POINT ( 'NONE',  ( 0.3124999999999996669, 0.1294417382415925521, 0.3209722222222261001 ) ) ;
#11591 = CARTESIAN_POINT ( 'NONE',  ( 0.3119999999999999996, 0.2402777777777774515, 0.000000000000000000 ) ) ;
#11592 = CARTESIAN_POINT ( 'NONE',  ( -0.1292346314604056745, 5.207027777777777366, -0.3119999999999999996 ) ) ;
#11593 = CARTESIAN_POINT ( 'NONE',  ( 0.1167790944451422702, 4.182722222298087544, -0.2819296736111110424 ) ) ;
#11594 = DIRECTION ( 'NONE',  ( -1.000000000000000000, 0.000000000000000000, 0.000000000000000000 ) ) ;
#11595 = CARTESIAN_POINT ( 'NONE',  ( -0.3257020783361852523, 0.3421021315173792821, 0.4271664148355318602 ) ) ;
#11596 = CARTESIAN_POINT ( 'NONE',  ( 0.06335377612981404893, 0.4070980611782420988, -0.4000000000000001887 ) ) ;
#11597 = ORIENTED_EDGE ( 'NONE', *, *, #10608, .F. ) ;
#11598 = CARTESIAN_POINT ( 'NONE',  ( 1.910449006669871087E-17, 0.3652777777777774237, -0.3119999999999999996 ) ) ;
#11599 = CARTESIAN_POINT ( 'NONE',  ( 0.1993543840281267465, 4.707027777853643791, 0.1993543840281266633 ) ) ;
#11600 = CARTESIAN_POINT ( 'NONE',  ( 0.3147071693084030897, -0.3721877333702315882, 0.07155713030921627416 ) ) ;
#11601 = CARTESIAN_POINT ( 'NONE',  ( 0.1294417382415924134, 0.3124999999999999445, -0.005416666666665343258 ) ) ;
#11602 = VECTOR ( 'NONE', #17760, 39.37007874015748143 ) ;
#11603 = CARTESIAN_POINT ( 'NONE',  ( 0.4802535697964960826, -0.2139886670027110471, 0.05346678874215700372 ) ) ;
#11604 = CARTESIAN_POINT ( 'NONE',  ( 0.000000000000000000, 0.2764156081756484196, -0.1477777777777777857 ) ) ;
#11605 = CARTESIAN_POINT ( 'NONE',  ( -0.1167790944451423119, 4.356333333409199149, -0.2819296736111110979 ) ) ;
#11606 = COORDINATED_UNIVERSAL_TIME_OFFSET ( 0, 0, .AHEAD. ) ;
#11607 = CARTESIAN_POINT ( 'NONE',  ( -0.3105842280018246138, 4.056716673947225793, -0.03562418879921332854 ) ) ;
#11608 = CARTESIAN_POINT ( 'NONE',  ( 2.352842711703412526, 2.664999999999999591, -2.591000000000000636 ) ) ;
#11609 = ORIENTED_EDGE ( 'NONE', *, *, #14593, .F. ) ;
#11610 = CARTESIAN_POINT ( 'NONE',  ( -0.1993543840281267465, 0.5284722221463555858, 0.1993543840281266633 ) ) ;
#11611 = LINE ( 'NONE', #13324, #9228 ) ;
#11612 = CARTESIAN_POINT ( 'NONE',  ( 2.575339694675500462E-17, 0.2749999999999999112, -0.4205848896953069405 ) ) ;
#11613 = CARTESIAN_POINT ( 'NONE',  ( -0.1306872919485614903, 0.3155070326520293400, 0.1074305555555573888 ) ) ;
#11614 = CARTESIAN_POINT ( 'NONE',  ( -0.3146687483788879192, -0.3722097299877869525, 0.07156199457777932815 ) ) ;
#11615 = CARTESIAN_POINT ( 'NONE',  ( -1.493307031895086562E-17, 0.6880286883367350281, -1.106874123228328788 ) ) ;
#11616 = CARTESIAN_POINT ( 'NONE',  ( -0.1167790944451424506, 0.4624999999241333759, 0.2819296736111110424 ) ) ;
#11617 = CARTESIAN_POINT ( 'NONE',  ( 0.2819296736111110424, 0.2541666665908000056, 0.1167790944451424923 ) ) ;
#11618 = ORIENTED_EDGE ( 'NONE', *, *, #975, .T. ) ;
#11619 = CARTESIAN_POINT ( 'NONE',  ( -1.726321361862525858E-17, 4.241750000075866112, -0.2819296736111110979 ) ) ;
#11620 = CIRCLE ( 'NONE', #21360, 0.4000000000000000222 ) ;
#11621 = CARTESIAN_POINT ( 'NONE',  ( -0.4000000000000000222, 0.3589285712334866485, 0.1299678784931624920 ) ) ;
#11622 = ADVANCED_FACE ( 'NONE', ( #6627 ), #10788, .F. ) ;
#11623 = CARTESIAN_POINT ( 'NONE',  ( 5.178964085587577574E-17, 4.825083333409199149, 0.2819296736111110979 ) ) ;
#11624 = ADVANCED_FACE ( 'NONE', ( #17856 ), #16023, .T. ) ;
#11625 = CARTESIAN_POINT ( 'NONE',  ( -0.1993543840281266910, 4.123694444520309865, -0.1993543840281266910 ) ) ;
#11626 = CARTESIAN_POINT ( 'NONE',  ( 1.286352214327351806, 2.291712385858714285, -1.542360493909560759 ) ) ;
#11627 = ORIENTED_EDGE ( 'NONE', *, *, #20163, .T. ) ;
#11628 = CARTESIAN_POINT ( 'NONE',  ( 0.000000000000000000, 5.384999999999999787, 0.000000000000000000 ) ) ;
#11629 = CARTESIAN_POINT ( 'NONE',  ( 0.3119999999999999996, 4.144527777929510215, -0.1292346314604056745 ) ) ;
#11630 = CARTESIAN_POINT ( 'NONE',  ( 2.500728763858895135E-17, 0.000000000000000000, -0.2041999999999999926 ) ) ;
#11631 = DIRECTION ( 'NONE',  ( 0.000000000000000000, -0.7071067811865475727, -0.7071067811865475727 ) ) ;
#11632 = ORIENTED_EDGE ( 'NONE', *, *, #17389, .F. ) ;
#11633 =( BOUNDED_CURVE ( )  B_SPLINE_CURVE ( 2, ( #6196, #8262, #6437, #12194, #22784, #21196, #2431, #20959, #9873 ),
 .UNSPECIFIED., .F., .F. ) 
 B_SPLINE_CURVE_WITH_KNOTS ( ( 3, 2, 2, 2, 3 ),
 ( 0.8125000000000000000, 0.8229166666666666297, 0.8333333333333333703, 0.8437500000000000000, 0.8541666666666666297 ),
 .UNSPECIFIED. ) 
 CURVE ( )  GEOMETRIC_REPRESENTATION_ITEM ( )  RATIONAL_B_SPLINE_CURVE ( ( 1.000000000000000000, 0.9238795325112867385, 1.000000000000000000, 0.9238795325112867385, 1.000000000000000000, 0.9238795325112867385, 1.000000000000000000, 0.9238795325112867385, 1.000000000000000000 ) ) 
 REPRESENTATION_ITEM ( '' )  );
#11634 = VECTOR ( 'NONE', #9440, 39.37007874015748854 ) ;
#11635 = APPLICATION_PROTOCOL_DEFINITION ( 'international standard', 'config_control_design', 1994, #8407 ) ;
#11636 = VERTEX_POINT ( 'NONE', #20404 ) ;
#11637 = CARTESIAN_POINT ( 'NONE',  ( 6.089848770316828444E-07, 4.238302053322364316, 0.3119999999987258521 ) ) ;
#11638 = CARTESIAN_POINT ( 'NONE',  ( -0.07934877013414777525, 5.013721278816293037, 0.3045045899376126464 ) ) ;
#11639 = EDGE_LOOP ( 'NONE', ( #4329, #10108, #4772, #22942 ) ) ;
#11640 = CARTESIAN_POINT ( 'NONE',  ( 0.1167790944451423257, 0.004166666590800036790, -0.2819296736111110424 ) ) ;
#11641 = ORIENTED_EDGE ( 'NONE', *, *, #17053, .T. ) ;
#11642 = LINE ( 'NONE', #413, #9345 ) ;
#11643 = FACE_OUTER_BOUND ( 'NONE', #588, .T. ) ;
#11644 = CARTESIAN_POINT ( 'NONE',  ( -0.3119999999999999996, 0.5458333333333329485, -3.820898013339742174E-17 ) ) ;
#11645 = CARTESIAN_POINT ( 'NONE',  ( -0.3613381517857143232, 0.02946428561674330898, -4.425116109941954795E-17 ) ) ;
#11646 = CARTESIAN_POINT ( 'NONE',  ( 0.2934911225613386909, 5.179109063580405348, -0.006257992997124091177 ) ) ;
#11647 = CC_DESIGN_PERSON_AND_ORGANIZATION_ASSIGNMENT ( #5533, #39, ( #2554 ) ) ;
#11648 = ORIENTED_EDGE ( 'NONE', *, *, #20695, .F. ) ;
#11649 = CARTESIAN_POINT ( 'NONE',  ( 0.3613381517857143232, 0.4401785713310289450, 0.000000000000000000 ) ) ;
#11650 = DIRECTION ( 'NONE',  ( -0.000000000000000000, 1.000000000000000000, -0.000000000000000000 ) ) ;
#11651 = CARTESIAN_POINT ( 'NONE',  ( 0.1144950937579611444, 0.2764156081756483641, 0.4043055555555599145 ) ) ;
#11652 = CARTESIAN_POINT ( 'NONE',  ( -1.726321361862525858E-17, 4.005638888964754507, -0.2819296736111110979 ) ) ;
#11653 = CARTESIAN_POINT ( 'NONE',  ( -0.5116234456863466562, 3.514980167629567998, 2.949589416182695878 ) ) ;
#11654 = CARTESIAN_POINT ( 'NONE',  ( 0.04000452085013941200, 5.119333780138143553, 0.3065892211030125658 ) ) ;
#11655 = CARTESIAN_POINT ( 'NONE',  ( -0.2909981737311249095, 5.180927869648259687, 0.03329044010142344356 ) ) ;
#11656 = AXIS2_PLACEMENT_3D ( 'NONE', #7, #1971, #22450 ) ;
#11657 = CARTESIAN_POINT ( 'NONE',  ( 0.3119999999999999996, 4.748694444596176290, 0.1292346314604056190 ) ) ;
#11658 = CARTESIAN_POINT ( 'NONE',  ( -0.1167790944451423119, 5.023000000075866112, -0.2819296736111110979 ) ) ;
#11659 = ORIENTED_EDGE ( 'NONE', *, *, #13409, .F. ) ;
#11660 = CARTESIAN_POINT ( 'NONE',  ( -0.2819296736111110424, 4.300777777853642903, 0.1167790944451424923 ) ) ;
#11661 = CARTESIAN_POINT ( 'NONE',  ( -0.3613381517857143232, 0.1723214284738861513, -4.425116109941954795E-17 ) ) ;
#11662 = ORIENTED_EDGE ( 'NONE', *, *, #5716, .T. ) ;
#11663 = EDGE_CURVE ( 'NONE', #5916, #22186, #2028, .T. ) ;
#11664 = ORIENTED_EDGE ( 'NONE', *, *, #23173, .T. ) ;
#11665 = CALENDAR_DATE ( 2026, 7, 10 ) ;
#11666 = DIRECTION ( 'NONE',  ( 1.000000000000000000, 0.000000000000000000, 0.000000000000000000 ) ) ;
#11667 = FACE_OUTER_BOUND ( 'NONE', #15368, .T. ) ;
#11668 = CARTESIAN_POINT ( 'NONE',  ( -0.1167790944451423535, 3.821611111186977272, 0.2819296736111110979 ) ) ;
#11669 = VECTOR ( 'NONE', #23359, 39.37007874015748143 ) ;
#11670 = CARTESIAN_POINT ( 'NONE',  ( 0.000000000000000000, 5.384999999999999787, 0.000000000000000000 ) ) ;
#11672 = ADVANCED_FACE ( 'NONE', ( #5403 ), #24049, .F. ) ;
#11671 = LINE ( 'NONE', #6895, #1517 ) ;
#11673 = CARTESIAN_POINT ( 'NONE',  ( 0.01172578639831966391, -0.5344959914317446437, 0.04874733047933994118 ) ) ;
#11674 = CARTESIAN_POINT ( 'NONE',  ( -0.2764156081756484196, 0.1144950937579609918, 0.3070833333333369830 ) ) ;
#11675 = CARTESIAN_POINT ( 'NONE',  ( -0.2819296736111110979, 0.5215277777019110550, -3.452642723725051716E-17 ) ) ;
#11676 = CARTESIAN_POINT ( 'NONE',  ( 0.2764156081756483641, -0.1144950937579611167, 0.4529166666666714636 ) ) ;
#11677 = ORIENTED_EDGE ( 'NONE', *, *, #14388, .T. ) ;
#11678 = CARTESIAN_POINT ( 'NONE',  ( -0.1993543840281266355, 4.651472222298087544, 0.1993543840281267465 ) ) ;
#11679 = CARTESIAN_POINT ( 'NONE',  ( -0.1292346314604057300, 3.950083333333332281, 0.3119999999999998885 ) ) ;
#11680 = CARTESIAN_POINT ( 'NONE',  ( 5.178964085587577574E-17, 4.755638888964754507, 0.2819296736111110979 ) ) ;
#11681 = CARTESIAN_POINT ( 'NONE',  ( -0.08061050724763124675, 4.157245614755926688, -0.3020926103485261915 ) ) ;
#11682 = CARTESIAN_POINT ( 'NONE',  ( 7.515426412127797749E-07, 4.849418923572540230, 0.3119999999980542227 ) ) ;
#11683 = CARTESIAN_POINT ( 'NONE',  ( -0.3875310796859931517, 2.665439728940003759E-18, 0.09388783919108294185 ) ) ;
#11684 = DIRECTION ( 'NONE',  ( -0.000000000000000000, -1.000000000000000000, -0.000000000000000000 ) ) ;
#11685 = CARTESIAN_POINT ( 'NONE',  ( -0.3119999999999999996, 4.269527777777777366, -0.1292346314604056468 ) ) ;
#11686 = CARTESIAN_POINT ( 'NONE',  ( -0.2472135954999579444, 0.2821428571428570287, -0.3402603233408160732 ) ) ;
#11687 = CARTESIAN_POINT ( 'NONE',  ( -0.2206173157302028787, 0.5458333331816004330, 0.2206173157302027954 ) ) ;
#11688 = AXIS2_PLACEMENT_3D ( 'NONE', #24050, #9306, #10789 ) ;
#11689 = ORIENTED_EDGE ( 'NONE', *, *, #18990, .F. ) ;
#11690 = CARTESIAN_POINT ( 'NONE',  ( 0.3108774165693796721, 4.584777046742110507, 0.02644302458017251320 ) ) ;
#11691 = ORIENTED_EDGE ( 'NONE', *, *, #22118, .T. ) ;
#11692 = CARTESIAN_POINT ( 'NONE',  ( 2.361207924709802342, 0.006657555934166073386, -2.942657555934166780 ) ) ;
#11693 = UNCERTAINTY_MEASURE_WITH_UNIT (LENGTH_MEASURE( 1.000000000000000082E-05 ), #9433, 'distance_accuracy_value', 'NONE');
#11694 = CARTESIAN_POINT ( 'NONE',  ( 0.1907340935051382025, 4.133015612144294693, 0.2469099182623766542 ) ) ;
#11695 = CARTESIAN_POINT ( 'NONE',  ( -0.1144950937579609918, -0.2764156081756484196, 0.4320833333333379822 ) ) ;
#11696 = CARTESIAN_POINT ( 'NONE',  ( 0.08154560721408028734, 4.296146448903024329, 0.3039036348046776359 ) ) ;
#11697 = EDGE_CURVE ( 'NONE', #6549, #21116, #7244, .T. ) ;
#11698 = ORIENTED_EDGE ( 'NONE', *, *, #3944, .T. ) ;
#11699 = CARTESIAN_POINT ( 'NONE',  ( -0.2233192592356399997, -0.03125000009754239083, 0.3073725909049499494 ) ) ;
#11700 = CONICAL_SURFACE ( 'NONE', #7016, 0.2500000000000000555, 0.5235987755984723435 ) ;
#11701 = CARTESIAN_POINT ( 'NONE',  ( 0.2819296736111110424, 0.3722222221463555858, -0.1167790944451423119 ) ) ;
#11702 = DIRECTION ( 'NONE',  ( 1.000000000000000000, 0.000000000000000000, 0.000000000000000000 ) ) ;
#11703 = CARTESIAN_POINT ( 'NONE',  ( 0.2988972802092635939, 0.3766541926404427532, -1.152205679622806622 ) ) ;
#11704 = CARTESIAN_POINT ( 'NONE',  ( -0.2887653152721422756, -0.08545421435185589221, -0.08979496337181655519 ) ) ;
#11705 = CARTESIAN_POINT ( 'NONE',  ( -3.385114897866767815E-17, -0.2764156081756484196, 0.2202777777777806811 ) ) ;
#11706 = CARTESIAN_POINT ( 'NONE',  ( -0.1528469870339583259, 4.622614882896163735, 0.2719999503001284125 ) ) ;
#11707 = CARTESIAN_POINT ( 'NONE',  ( 0.000000000000000000, 3.738758431839877614E-19, 0.4425000000000000044 ) ) ;
#11708 = CARTESIAN_POINT ( 'NONE',  ( -0.1474902928972388061, -2.846948999568498288E-18, -0.3603575498838690883 ) ) ;
#11709 = CARTESIAN_POINT ( 'NONE',  ( -0.3119999999999999996, 0.1534722222222218990, -0.1292346314604056745 ) ) ;
#11710 = CARTESIAN_POINT ( 'NONE',  ( 0.1292346314604058410, 5.179249999999998799, 0.3119999999999998885 ) ) ;
#11711 = CARTESIAN_POINT ( 'NONE',  ( 0.2819296736111110979, 4.113277777853643791, 0.1167790944451422425 ) ) ;
#11712 = CARTESIAN_POINT ( 'NONE',  ( 0.000000000000000000, 0.02999999999999995379, 0.3425000000000000266 ) ) ;
#11713 = CARTESIAN_POINT ( 'NONE',  ( -0.2676934969451049695, 0.3758505236666521698, 0.4334994210334168208 ) ) ;
#11714 = CARTESIAN_POINT ( 'NONE',  ( -0.3866234456863257840, 3.706421428007541596, -2.712949941383575592 ) ) ;
#11715 = ORIENTED_EDGE ( 'NONE', *, *, #13818, .T. ) ;
#11716 = CARTESIAN_POINT ( 'NONE',  ( -0.1294417382415922746, -0.3125000000000000000, 0.1334722222222246568 ) ) ;
#11717 = CARTESIAN_POINT ( 'NONE',  ( -1.726321361862525858E-17, 4.672305555631421470, -0.2819296736111110979 ) ) ;
#11718 = CARTESIAN_POINT ( 'NONE',  ( 0.01848103877824576122, 0.5441716683897390716, 0.04413116910601656839 ) ) ;
#11719 = AXIS2_PLACEMENT_3D ( 'NONE', #16019, #13956, #13723 ) ;
#11720 = CARTESIAN_POINT ( 'NONE',  ( -0.03098226891380893508, 4.515206242287482574, 0.3104630823214994950 ) ) ;
#11721 = EDGE_CURVE ( 'NONE', #5324, #16705, #604, .T. ) ;
#11722 = CIRCLE ( 'NONE', #1192, 0.01874999999999999237 ) ;
#11723 = EDGE_CURVE ( 'NONE', #12731, #18391, #15246, .T. ) ;
#11724 = DIRECTION ( 'NONE',  ( -0.1474777632191348331, -0.6043296738907314447, -0.7829661260942282208 ) ) ;
#11725 = CARTESIAN_POINT ( 'NONE',  ( 0.3119999999999999996, 0.6256944442927114824, -0.1292346314604056468 ) ) ;
#11726 = CARTESIAN_POINT ( 'NONE',  ( -0.1993543840281266355, 4.318138888964754507, 0.1993543840281267465 ) ) ;
#11727 = PERSON_AND_ORGANIZATION ( #10300, #20880 ) ;
#11728 = EDGE_CURVE ( 'NONE', #7491, #6190, #5965, .T. ) ;
#11729 = CARTESIAN_POINT ( 'NONE',  ( -0.2670672243593699702, 4.052874141853025414, -0.1660684718339069943 ) ) ;
#11730 = CARTESIAN_POINT ( 'NONE',  ( -3.385114897866767815E-17, -0.2764156081756484196, -0.05749999999999930167 ) ) ;
#11731 = CYLINDRICAL_SURFACE ( 'NONE', #23476, 0.3119999999999999996 ) ;
#11732 = ORIENTED_EDGE ( 'NONE', *, *, #4570, .T. ) ;
#11733 = CARTESIAN_POINT ( 'NONE',  ( 0.2819296736111110424, 0.4902777777019112215, 0.1167790944451424923 ) ) ;
#11734 = CARTESIAN_POINT ( 'NONE',  ( 0.1292346314604058410, 4.123694444444444329, 0.3119999999999998885 ) ) ;
#11735 = DIRECTION ( 'NONE',  ( -0.000000000000000000, -1.000000000000000000, -0.000000000000000000 ) ) ;
#11736 = CARTESIAN_POINT ( 'NONE',  ( 0.3125000000000000000, -5.740531871003217465E-17, -0.02277777777777697382 ) ) ;
#11737 = CARTESIAN_POINT ( 'NONE',  ( -0.1306872919485614903, 0.3155070326520293400, 0.2185416666666694097 ) ) ;
#11738 = DIRECTION ( 'NONE',  ( -0.000000000000000000, -1.000000000000000000, -0.000000000000000000 ) ) ;
#11739 = CARTESIAN_POINT ( 'NONE',  ( 0.3119999999999999996, 5.026472222222221120, -0.1292346314604056745 ) ) ;
#11740 = CARTESIAN_POINT ( 'NONE',  ( -0.2819296736111111534, 0.4555555554796890116, 0.1167790944451422563 ) ) ;
#11741 = CARTESIAN_POINT ( 'NONE',  ( -0.1993543840281266633, 0.2229166665908000333, -0.1993543840281266910 ) ) ;
#11742 = ORIENTED_EDGE ( 'NONE', *, *, #7094, .T. ) ;
#11743 = AXIS2_PLACEMENT_3D ( 'NONE', #24028, #9045, #5382 ) ;
#11744 = CARTESIAN_POINT ( 'NONE',  ( 0.2819296736111110979, 4.224388888964755395, 0.1167790944451422425 ) ) ;
#11745 = CARTESIAN_POINT ( 'NONE',  ( 0.4000000000000000222, 0.2482142855192009112, 0.000000000000000000 ) ) ;
#11746 = CARTESIAN_POINT ( 'NONE',  ( 0.2819296736111110979, 4.894527777853643791, -3.452642723725051716E-17 ) ) ;
#11747 = CARTESIAN_POINT ( 'NONE',  ( -1.726321361862525858E-17, 4.283416666742532186, -0.2819296736111110979 ) ) ;
#11748 = DIRECTION ( 'NONE',  ( -0.3895442144046399879, 0.7839133596588501174, 0.4834616319546425900 ) ) ;
#11749 = EDGE_LOOP ( 'NONE', ( #19370, #18922, #7892, #6425, #17936, #17132, #15451 ) ) ;
#11750 = CARTESIAN_POINT ( 'NONE',  ( 0.1294417382415924134, 0.3124999999999999445, 0.09875000000000175304 ) ) ;
#11751 = CARTESIAN_POINT ( 'NONE',  ( -1.910449006669871087E-17, 3.932722222373954413, -0.3119999999999999996 ) ) ;
#11752 = CARTESIAN_POINT ( 'NONE',  ( -5.731347020009612645E-17, 0.1152777777777774515, 0.3119999999999999996 ) ) ;
#11753 = CARTESIAN_POINT ( 'NONE',  ( 0.1484667313406524691, -0.2653928060426358204, -0.09280364848304442638 ) ) ;
#11754 = ORIENTED_EDGE ( 'NONE', *, *, #1278, .T. ) ;
#11755 = EDGE_CURVE ( 'NONE', #428, #412, #19120, .T. ) ;
#11756 = COORDINATED_UNIVERSAL_TIME_OFFSET ( 0, 0, .AHEAD. ) ;
#11757 = FACE_OUTER_BOUND ( 'NONE', #3476, .T. ) ;
#11758 = CARTESIAN_POINT ( 'NONE',  ( -0.3566234456863258129, 4.730490217694244492, -2.730270449459264004 ) ) ;
#11759 = ORIENTED_EDGE ( 'NONE', *, *, #13694, .T. ) ;
#11760 = CARTESIAN_POINT ( 'NONE',  ( 0.2206173157302027676, 0.6152777776260449638, 0.2206173157302028787 ) ) ;
#11761 = ORIENTED_EDGE ( 'NONE', *, *, #23603, .F. ) ;
#11762 = CARTESIAN_POINT ( 'NONE',  ( 0.2837750196973463646, 4.255964866207376573, -0.1296761943110192605 ) ) ;
#11763 = DIRECTION ( 'NONE',  ( 1.000000000000000000, 0.000000000000000000, 0.000000000000000000 ) ) ;
#11764 = CARTESIAN_POINT ( 'NONE',  ( 0.9125529719201093126, 2.740000000000000213, -1.580588111963586062 ) ) ;
#11765 = CARTESIAN_POINT ( 'NONE',  ( 2.326421213736078119E-17, 0.08303571418817184968, -0.3799334167787516425 ) ) ;
#11766 = CARTESIAN_POINT ( 'NONE',  ( 0.07599768514248278484, 5.169247371546412673, 0.2875240573393413879 ) ) ;
#11767 = ORIENTED_EDGE ( 'NONE', *, *, #11870, .F. ) ;
#11768 = CARTESIAN_POINT ( 'NONE',  ( -0.2233192592356400275, 0.4151785713310289228, 0.3073725909049499494 ) ) ;
#11769 = ORIENTED_EDGE ( 'NONE', *, *, #20202, .F. ) ;
#11770 = CARTESIAN_POINT ( 'NONE',  ( 0.2764156081756483641, 0.1144950937579610056, 0.4529166666666715191 ) ) ;
#11771 = CARTESIAN_POINT ( 'NONE',  ( 0.1993543840281266633, 3.943138888964754507, -0.1993543840281266910 ) ) ;
#11772 = CARTESIAN_POINT ( 'NONE',  ( -0.4581189881604794123, -0.2644951211353319120, 0.3941886329748525153 ) ) ;
#11773 = CARTESIAN_POINT ( 'NONE',  ( -0.1211763616584382586, 5.192648849054667615, 0.2616024314742874113 ) ) ;
#11774 = CARTESIAN_POINT ( 'NONE',  ( -1.910449006669871087E-17, 4.432722222373953969, -0.3119999999999999996 ) ) ;
#11775 = CARTESIAN_POINT ( 'NONE',  ( 0.1167790944451424506, 4.939666666742532186, 0.2819296736111110424 ) ) ;
#11776 = VERTEX_POINT ( 'NONE', #17196 ) ;
#11777 = CARTESIAN_POINT ( 'NONE',  ( 0.2819296736111110979, 4.380638888964754507, -3.452642723725051716E-17 ) ) ;
#11778 = CARTESIAN_POINT ( 'NONE',  ( -0.3613381517857143232, 0.3116071427596003862, -0.1174058825155741143 ) ) ;
#11779 = VERTEX_POINT ( 'NONE', #14809 ) ;
#11780 = ORIENTED_EDGE ( 'NONE', *, *, #3305, .T. ) ;
#11781 = APPROVAL_ROLE ( '' ) ;
#11782 = DIRECTION ( 'NONE',  ( 0.000000000000000000, 0.000000000000000000, 1.000000000000000000 ) ) ;
#11783 = DIRECTION ( 'NONE',  ( 0.000000000000000000, 0.000000000000000000, -1.000000000000000000 ) ) ;
#11784 = CARTESIAN_POINT ( 'NONE',  ( -0.2819296736111110979, 3.752166666742532630, -0.1167790944451422980 ) ) ;
#11785 = CARTESIAN_POINT ( 'NONE',  ( 0.07355958478172115733, 4.407018638961537782, 0.3032090396793259424 ) ) ;
#11786 = CARTESIAN_POINT ( 'NONE',  ( -0.2209708691207961373, -0.2209708691207961095, -0.09222222222222160870 ) ) ;
#11787 = CARTESIAN_POINT ( 'NONE',  ( 0.3103970466387488414, -0.3620580589327280219, 0.08855978515307991183 ) ) ;
#11788 = CARTESIAN_POINT ( 'NONE',  ( -0.2764156081756484196, 1.692557448933383907E-17, 0.2550000000000032241 ) ) ;
#11789 = CARTESIAN_POINT ( 'NONE',  ( -0.1993543840281266633, 0.5701388888130222155, -0.1993543840281266910 ) ) ;
#11790 = CARTESIAN_POINT ( 'NONE',  ( -0.2764156081756484196, 0.1144950937579609918, -0.08180555555555503455 ) ) ;
#11791 = VERTEX_POINT ( 'NONE', #16510 ) ;
#11792 = CARTESIAN_POINT ( 'NONE',  ( 0.1993543840281267465, 4.776472222298088433, 0.1993543840281266633 ) ) ;
#11793 = DIRECTION ( 'NONE',  ( 0.000000000000000000, 0.000000000000000000, -1.000000000000000000 ) ) ;
#11794 = VECTOR ( 'NONE', #15100, 39.37007874015748143 ) ;
#11795 = CARTESIAN_POINT ( 'NONE',  ( -1.726321361862525858E-17, 4.616750000075865223, -0.2819296736111110979 ) ) ;
#11796 = CARTESIAN_POINT ( 'NONE',  ( 0.4584481579615881097, -0.2211256433011207223, 0.4059661290276580514 ) ) ;
#11797 =( BOUNDED_CURVE ( )  B_SPLINE_CURVE ( 2, ( #18925, #2461, #4279, #11859, #19274, #20746, #2224, #11734, #17094 ),
 .UNSPECIFIED., .F., .F. ) 
 B_SPLINE_CURVE_WITH_KNOTS ( ( 3, 2, 2, 2, 3 ),
 ( 0.7232142857142858094, 0.7276785714285715079, 0.7321428571428572063, 0.7366071428571429047, 0.7410714285714286031 ),
 .UNSPECIFIED. ) 
 CURVE ( )  GEOMETRIC_REPRESENTATION_ITEM ( )  RATIONAL_B_SPLINE_CURVE ( ( 0.9999999999999981126, 0.9238795325112886259, 1.000000000000000000, 0.9238795325112867385, 1.000000000000000000, 0.9238795325112867385, 1.000000000000000000, 0.9238795325112867385, 1.000000000000000000 ) ) 
 REPRESENTATION_ITEM ( '' )  );
#11798 = EDGE_CURVE ( 'NONE', #4141, #11248, #3934, .T. ) ;
#11799 = CARTESIAN_POINT ( 'NONE',  ( 0.04546508165698102955, 4.850751077471080919, 0.3093939345129879115 ) ) ;
#11800 = DIRECTION ( 'NONE',  ( 0.000000000000000000, 0.000000000000000000, -1.000000000000000000 ) ) ;
#11801 = DIRECTION ( 'NONE',  ( 0.000000000000000000, 0.000000000000000000, 1.000000000000000000 ) ) ;
#11802 = CARTESIAN_POINT ( 'NONE',  ( -1.910449006669871087E-17, 4.203555555555555046, -0.3119999999999999996 ) ) ;
#11803 = CARTESIAN_POINT ( 'NONE',  ( 0.000000000000000000, 3.738758431839877614E-19, 0.4241666666666665253 ) ) ;
#11804 = ADVANCED_FACE ( 'NONE', ( #13427, #3572 ), #4139, .F. ) ;
#11805 = CARTESIAN_POINT ( 'NONE',  ( 0.1292346314604058410, 5.186194444596176290, 0.3119999999999998885 ) ) ;
#11806 = CARTESIAN_POINT ( 'NONE',  ( 0.3003475124358454540, 1.999640111863030256, -3.545613612297686679 ) ) ;
#11807 = ORIENTED_EDGE ( 'NONE', *, *, #5712, .T. ) ;
#11808 = DIMENSIONAL_EXPONENTS ( 1.000000000000000000, 0.000000000000000000, 0.000000000000000000, 0.000000000000000000, 0.000000000000000000, 0.000000000000000000, 0.000000000000000000 ) ;
#11809 = CARTESIAN_POINT ( 'NONE',  ( 0.3124999999999993339, 0.1294417382415928297, 0.2029166666666692709 ) ) ;
#11810 = EDGE_LOOP ( 'NONE', ( #21875, #19814, #16010, #1263 ) ) ;
#11811 = APPROVAL ( #14058, 'UNSPECIFIED' ) ;
#11812 = EDGE_CURVE ( 'NONE', #14200, #12633, #23770, .T. ) ;
#11813 = CARTESIAN_POINT ( 'NONE',  ( 0.006135078556594095005, 4.710334877597526670, -0.3119484483264631236 ) ) ;
#11814 = VECTOR ( 'NONE', #9454, 39.37007874015748143 ) ;
#11815 = CARTESIAN_POINT ( 'NONE',  ( 0.1873983838916965794, 4.132896614991455664, 0.2494675077111220274 ) ) ;
#11816 = CARTESIAN_POINT ( 'NONE',  ( 0.000000000000000000, 0.3155070326520292845, -0.1703472222222222054 ) ) ;
#11817 = B_SPLINE_CURVE_WITH_KNOTS ( 'NONE', 3,
 ( #14706, #14825, #9931, #9685, #4306, #21378, #22843, #8202, #8080, #2723, #19183, #9811, #6132, #2375, #22722, #23070, #19307, #11520, #2251, #6379, #2610, #10054, #21136, #17599, #17478, #6500, #8320, #11762, #15415, #770, #13599, #6256, #10177, #890, #15772, #17124, #13950, #4425, #11891, #21012, #22953, #15651, #13827, #23191 ),
 .UNSPECIFIED., .F., .F.,
 ( 4, 2, 1, 1, 1, 1, 1, 1, 2, 2, 2, 2, 2, 2, 2, 2, 2, 2, 1, 1, 2, 2, 2, 2, 2, 4 ),
 ( 0.6304885228263440444, 0.6304929868432944673, 0.6304974508602450012, 0.6305063788941459579, 0.6305242349619478714, 0.6305599470975516985, 0.6306313713687593525, 0.6307742199111745496, 0.6310599169960051658, 0.6316313111656661761, 0.6327740995049883077, 0.6339168878443105504, 0.6350596761836326820, 0.6362024645229548137, 0.6367738586926158240, 0.6370595557774464401, 0.6371309800486540942, 0.6371488361164560077, 0.6371666921842579212, 0.6372024043198616372, 0.6373452528622769453, 0.6396308295409212086, 0.6419164062195654719, 0.6442019828982096241, 0.6464875595768538874, 0.6487731362554981507 ),
 .UNSPECIFIED. ) ;
#11818 = VERTEX_POINT ( 'NONE', #13554 ) ;
#11819 = CARTESIAN_POINT ( 'NONE',  ( 0.3037735703191254411, 4.305353122071822192, 0.08207324121115516791 ) ) ;
#11820 = ORIENTED_EDGE ( 'NONE', *, *, #20953, .T. ) ;
#11821 = CARTESIAN_POINT ( 'NONE',  ( -0.3613381517857143232, 0.02946428561674330898, -4.425116109941954795E-17 ) ) ;
#11822 = CARTESIAN_POINT ( 'NONE',  ( -0.2819296736111110979, 0.5666666665908001166, 0.1167790944451422425 ) ) ;
#11823 = CARTESIAN_POINT ( 'NONE',  ( -0.3125000000000000000, 1.913510623667739771E-17, 0.4008333333333378712 ) ) ;
#11824 = CARTESIAN_POINT ( 'NONE',  ( -0.07165243469752499705, -0.2702856358549580174, -0.06824753933085654645 ) ) ;
#11825 = CARTESIAN_POINT ( 'NONE',  ( -0.1954553509668046918, -0.1954553509668046640, 0.2688888888888921747 ) ) ;
#11826 = ORIENTED_EDGE ( 'NONE', *, *, #6913, .F. ) ;
#11827 = DIRECTION ( 'NONE',  ( -0.000000000000000000, -1.000000000000000000, -0.000000000000000000 ) ) ;
#11828 = EDGE_CURVE ( 'NONE', #22848, #14521, #13209, .T. ) ;
#11829 = CARTESIAN_POINT ( 'NONE',  ( 0.4959544880677846934, 2.765954488067785100, -0.6103003506586756055 ) ) ;
#11830 = CARTESIAN_POINT ( 'NONE',  ( 0.5097595264191659981, 2.690047770615767941, -0.7016051277422445942 ) ) ;
#11831 = CARTESIAN_POINT ( 'NONE',  ( -0.2206173157302027954, 0.1499999999999996336, -0.2206173157302028232 ) ) ;
#11832 = CARTESIAN_POINT ( 'NONE',  ( 0.1292346314604058410, 4.845916666666666650, 0.3119999999999998885 ) ) ;
#11833 = EDGE_CURVE ( 'NONE', #13967, #6423, #9187, .T. ) ;
#11834 = VECTOR ( 'NONE', #19495, 39.37007874015748143 ) ;
#11835 = CARTESIAN_POINT ( 'NONE',  ( -0.2819296736111110424, 3.918833333409198705, -0.1167790944451423119 ) ) ;
#11836 = CARTESIAN_POINT ( 'NONE',  ( 0.000000000000000000, 5.384999999999999787, -0.3119999999999999996 ) ) ;
#11837 = CARTESIAN_POINT ( 'NONE',  ( -0.2206173157302028232, 3.877166666666666206, -0.2206173157302028232 ) ) ;
#11838 = CARTESIAN_POINT ( 'NONE',  ( 0.03502586135503213405, 4.820592410594939814, -0.3119999852544549923 ) ) ;
#11839 = ORIENTED_EDGE ( 'NONE', *, *, #18713, .T. ) ;
#11840 = ORIENTED_EDGE ( 'NONE', *, *, #18463, .T. ) ;
#11841 = SPHERICAL_SURFACE ( 'NONE', #14392, 0.3119999999999999996 ) ;
#11842 = CARTESIAN_POINT ( 'NONE',  ( 5.178964085587577574E-17, 4.700083333409199149, 0.2819296736111110979 ) ) ;
#11843 = EDGE_CURVE ( 'NONE', #22186, #175, #4707, .T. ) ;
#11844 = CARTESIAN_POINT ( 'NONE',  ( 0.009374999999999683933, 0.5358532185916218271, 0.06112444011295371793 ) ) ;
#11845 = CARTESIAN_POINT ( 'NONE',  ( 0.3291860208797072196, -0.3512102395969137758, 0.4108348780186337201 ) ) ;
#11846 =( BOUNDED_SURFACE ( )  B_SPLINE_SURFACE ( 1, 2, ( 
 ( #24066, #14827, #22243, #12644, #22361, #16999, #9688, #22486, #14940, #3955, #5782, #292, #13244, #7732, #11281, #21015, #3839, #20898, #171, #9446, #4192, #19186, #11523, #16765, #17127, #4069, #15418, #15178, #11399, #13483, #11645, #16880, #22614, #13602, #48, #7967, #6015, #5664, #20544, #18956, #5899, #15298, #2254, #22846, #22725, #11765, #4309, #9566, #20659, #2126, #13128, #18711, #19070, #6135, #13357, #2009, #18831, #416, #7849, #20778, #2378, #9814, #2495, #17247, #531, #7494, #7612, #15064, #4911, #6259, #1138, #10422, #893, #14069, #6382, #8446, #19428, #15534, #17603, #13953, #10298, #23311, #23432, #14184, #8205, #13831, #6618, #21263, #15654, #8324, #4671, #15891, #4553, #6740, #4428, #19791, #21618, #17847, #21496, #9934, #22957, #12373, #17363, #15776, #655, #8573, #4785, #12015, #19547, #21139, #12253, #17722, #8083, #13719, #19668, #1016, #23073, #2726, #11895, #10180, #12140, #19310, #2613, #773, #2839, #6503, #23194, #10057, #17481, #21381, #2966, #16014, #21741, #9052, #18202, #5145, #10647, #12736, #3441, #16617, #22213 ),
 ( #3560, #22095, #24036, #12612, #1618, #12491, #8933, #1257, #20030, #8686, #7231, #3319, #10892, #12975, #10776, #21974, #5391, #3201, #6988, #14307, #11011, #16257, #5513, #20152, #3090, #1498, #16379, #1734, #23790, #18320, #14550, #18079, #5026, #7110, #19912, #10533, #5267, #14430, #16498, #23910, #14676, #12856, #8808, #20273, #18439, #9173, #7346, #14798, #17967, #16134, #1379, #23550, #6864, #23669, #21856, #7703, #15388, #13099, #22816, #18559, #140, #13217, #2093, #17216, #14911, #7583, #7934, #22695, #14, #15150, #4040, #11253, #11371, #22579, #17096, #263, #382, #5867, #7822, #18798, #1849, #20627, #6106, #5633, #18677, #9535, #13326, #15268, #20748, #5986, #11493, #13450, #16968, #9292, #3926, #20392, #20512, #9784, #18928, #11131, #4162, #20868, #15033, #2226, #7462, #11612, #9657, #3684, #16733, #19044, #2346, #1978, #5756, #22331, #500, #3807, #9416, #16853, #22457, #15748, #10149, #8173, #4281, #8538, #20985, #1104, #745, #8058, #19517, #4523, #15627, #21110, #23159, #13923, #2933, #15979, #15506, #19399, #6469, #15861, #11986 ) ),
 .UNSPECIFIED., .F., .F., .F. ) 
 B_SPLINE_SURFACE_WITH_KNOTS ( ( 2, 2 ),
 ( 3, 2, 2, 2, 2, 2, 2, 2, 2, 2, 2, 2, 2, 2, 2, 2, 2, 2, 2, 2, 2, 2, 2, 2, 2, 2, 2, 2, 2, 2, 2, 2, 2, 2, 2, 2, 2, 2, 2, 2, 2, 2, 2, 2, 2, 2, 2, 2, 2, 2, 2, 2, 2, 2, 2, 2, 2, 2, 2, 2, 2, 2, 2, 2, 2, 2, 2, 2, 2, 2, 3 ),
 ( 0.000000000000000000, 1.000000000000000000 ),
 ( 0.000000000000000000, 0.01428571428571428527, 0.02857142857142857054, 0.04285714285714285754, 0.05714285714285714107, 0.07142857142857142461, 0.08571428571428571508, 0.1000000000000000056, 0.1142857142857142821, 0.1285714285714285587, 0.1428571428571428492, 0.1571428571428571397, 0.1714285714285714302, 0.1857142857142857206, 0.2000000000000000111, 0.2142857142857142738, 0.2285714285714285643, 0.2428571428571428548, 0.2571428571428571175, 0.2714285714285714080, 0.2857142857142856984, 0.2999999999999999889, 0.3142857142857142794, 0.3285714285714285698, 0.3428571428571428603, 0.3571428571428571508, 0.3714285714285714413, 0.3857142857142857317, 0.4000000000000000222, 0.4142857142857143127, 0.4285714285714285476, 0.4428571428571428381, 0.4571428571428571286, 0.4714285714285714191, 0.4857142857142857095, 0.5000000000000000000, 0.5142857142857142350, 0.5285714285714285809, 0.5428571428571428159, 0.5571428571428571619, 0.5714285714285713969, 0.5857142857142857428, 0.5999999999999999778, 0.6142857142857143238, 0.6285714285714285587, 0.6428571428571429047, 0.6571428571428571397, 0.6714285714285713746, 0.6857142857142857206, 0.6999999999999999556, 0.7142857142857143016, 0.7285714285714285365, 0.7428571428571428825, 0.7571428571428571175, 0.7714285714285714635, 0.7857142857142856984, 0.8000000000000000444, 0.8142857142857142794, 0.8285714285714286254, 0.8428571428571428603, 0.8571428571428570953, 0.8714285714285714413, 0.8857142857142856762, 0.9000000000000000222, 0.9142857142857142572, 0.9285714285714286031, 0.9428571428571428381, 0.9571428571428571841, 0.9714285714285714191, 0.9857142857142857650, 1.000000000000000000 ),
 .UNSPECIFIED. ) 
 GEOMETRIC_REPRESENTATION_ITEM ( )  RATIONAL_B_SPLINE_SURFACE ( (
 ( 1.000000000000000000, 0.9510565162951535312, 1.000000000000000000, 0.9510565162951535312, 1.000000000000000000, 0.9510565162951535312, 1.000000000000000000, 0.9510565162951535312, 1.000000000000000000, 0.9510565162951535312, 1.000000000000000000, 0.9510565162951535312, 1.000000000000000000, 0.9510565162951535312, 1.000000000000000000, 0.9510565162951535312, 1.000000000000000000, 0.9510565162951535312, 1.000000000000000000, 0.9510565162951535312, 1.000000000000000000, 0.9510565162951535312, 1.000000000000000000, 0.9510565162951535312, 1.000000000000000000, 0.9510565162951535312, 1.000000000000000000, 0.9510565162951535312, 1.000000000000000000, 0.9510565162951535312, 1.000000000000000000, 0.9510565162951535312, 1.000000000000000000, 0.9510565162951535312, 1.000000000000000000, 0.9510565162951535312, 1.000000000000000000, 0.9510565162951535312, 1.000000000000000000, 0.9510565162951535312, 1.000000000000000000, 0.9510565162951535312, 1.000000000000000000, 0.9510565162951535312, 1.000000000000000000, 0.9510565162951535312, 1.000000000000000000, 0.9510565162951535312, 1.000000000000000000, 0.9510565162951535312, 1.000000000000000000, 0.9510565162951535312, 1.000000000000000000, 0.9510565162951535312, 1.000000000000000000, 0.9510565162951535312, 1.000000000000000000, 0.9510565162951535312, 1.000000000000000000, 0.9510565162951535312, 1.000000000000000000, 0.9510565162951535312, 1.000000000000000000, 0.9510565162951535312, 1.000000000000000000, 0.9510565162951535312, 1.000000000000000000, 0.9510565162951535312, 1.000000000000000000, 0.9510565162951535312, 1.000000000000000000, 0.9510565162951535312, 1.000000000000000000, 0.9510565162951535312, 1.000000000000000000, 0.9510565162951535312, 1.000000000000000000, 0.9510565162951535312, 1.000000000000000000, 0.9510565162951535312, 1.000000000000000000, 0.9510565162951535312, 1.000000000000000000, 0.9510565162951535312, 1.000000000000000000, 0.9510565162951535312, 1.000000000000000000, 0.9510565162951535312, 1.000000000000000000, 0.9510565162951535312, 1.000000000000000000, 0.9510565162951535312, 1.000000000000000000, 0.9510565162951535312, 1.000000000000000000, 0.9510565162951535312, 1.000000000000000000, 0.9510565162951535312, 1.000000000000000000, 0.9510565162951535312, 1.000000000000000000, 0.9510565162951535312, 1.000000000000000000, 0.9510565162951535312, 1.000000000000000000, 0.9510565162951535312, 1.000000000000000000, 0.9510565162951535312, 1.000000000000000000, 0.9510565162951535312, 1.000000000000000000, 0.9510565162951535312, 1.000000000000000000, 0.9510565162951535312, 1.000000000000000000, 0.9510565162951535312, 1.000000000000000000, 0.9510565162951535312, 1.000000000000000000, 0.9510565162951535312, 1.000000000000000000, 0.9510565162951535312, 1.000000000000000000, 0.9510565162951535312, 1.000000000000000000, 0.9510565162951535312, 1.000000000000000000, 0.9510565162951535312, 1.000000000000000000, 0.9510565162951535312, 1.000000000000000000, 0.9510565162951535312, 1.000000000000000000, 0.9510565162951535312, 1.000000000000000000, 0.9510565162951535312, 1.000000000000000000, 0.9510565162951535312, 1.000000000000000000, 0.9510565162951535312, 1.000000000000000000),
 ( 1.000000000000000000, 0.9510565162951535312, 1.000000000000000000, 0.9510565162951535312, 1.000000000000000000, 0.9510565162951535312, 1.000000000000000000, 0.9510565162951535312, 1.000000000000000000, 0.9510565162951535312, 1.000000000000000000, 0.9510565162951535312, 1.000000000000000000, 0.9510565162951535312, 1.000000000000000000, 0.9510565162951535312, 1.000000000000000000, 0.9510565162951535312, 1.000000000000000000, 0.9510565162951535312, 1.000000000000000000, 0.9510565162951535312, 1.000000000000000000, 0.9510565162951535312, 1.000000000000000000, 0.9510565162951535312, 1.000000000000000000, 0.9510565162951535312, 1.000000000000000000, 0.9510565162951535312, 1.000000000000000000, 0.9510565162951535312, 1.000000000000000000, 0.9510565162951535312, 1.000000000000000000, 0.9510565162951535312, 1.000000000000000000, 0.9510565162951535312, 1.000000000000000000, 0.9510565162951535312, 1.000000000000000000, 0.9510565162951535312, 1.000000000000000000, 0.9510565162951535312, 1.000000000000000000, 0.9510565162951535312, 1.000000000000000000, 0.9510565162951535312, 1.000000000000000000, 0.9510565162951535312, 1.000000000000000000, 0.9510565162951535312, 1.000000000000000000, 0.9510565162951535312, 1.000000000000000000, 0.9510565162951535312, 1.000000000000000000, 0.9510565162951535312, 1.000000000000000000, 0.9510565162951535312, 1.000000000000000000, 0.9510565162951535312, 1.000000000000000000, 0.9510565162951535312, 1.000000000000000000, 0.9510565162951535312, 1.000000000000000000, 0.9510565162951535312, 1.000000000000000000, 0.9510565162951535312, 1.000000000000000000, 0.9510565162951535312, 1.000000000000000000, 0.9510565162951535312, 1.000000000000000000, 0.9510565162951535312, 1.000000000000000000, 0.9510565162951535312, 1.000000000000000000, 0.9510565162951535312, 1.000000000000000000, 0.9510565162951535312, 1.000000000000000000, 0.9510565162951535312, 1.000000000000000000, 0.9510565162951535312, 1.000000000000000000, 0.9510565162951535312, 1.000000000000000000, 0.9510565162951535312, 1.000000000000000000, 0.9510565162951535312, 1.000000000000000000, 0.9510565162951535312, 1.000000000000000000, 0.9510565162951535312, 1.000000000000000000, 0.9510565162951535312, 1.000000000000000000, 0.9510565162951535312, 1.000000000000000000, 0.9510565162951535312, 1.000000000000000000, 0.9510565162951535312, 1.000000000000000000, 0.9510565162951535312, 1.000000000000000000, 0.9510565162951535312, 1.000000000000000000, 0.9510565162951535312, 1.000000000000000000, 0.9510565162951535312, 1.000000000000000000, 0.9510565162951535312, 1.000000000000000000, 0.9510565162951535312, 1.000000000000000000, 0.9510565162951535312, 1.000000000000000000, 0.9510565162951535312, 1.000000000000000000, 0.9510565162951535312, 1.000000000000000000, 0.9510565162951535312, 1.000000000000000000, 0.9510565162951535312, 1.000000000000000000, 0.9510565162951535312, 1.000000000000000000, 0.9510565162951535312, 1.000000000000000000, 0.9510565162951535312, 1.000000000000000000, 0.9510565162951535312, 1.000000000000000000, 0.9510565162951535312, 1.000000000000000000, 0.9510565162951535312, 1.000000000000000000, 0.9510565162951535312, 1.000000000000000000) ) ) 
 REPRESENTATION_ITEM ( '' )  SURFACE ( )  );
#11847 = PERSON_AND_ORGANIZATION ( #15518, #2538 ) ;
#11848 = CARTESIAN_POINT ( 'NONE',  ( 0.2694453590030795320, 0.3748737188716305679, 0.4343212420608417168 ) ) ;
#11849 = CARTESIAN_POINT ( 'NONE',  ( -0.1144950937579609918, -0.2764156081756484196, -0.1234722222222220528 ) ) ;
#11850 = CARTESIAN_POINT ( 'NONE',  ( 2.168722887430706070, 2.291712385858714729, -1.763529041877836212 ) ) ;
#11851 = CARTESIAN_POINT ( 'NONE',  ( -0.1993543840281266910, 4.304250000075866112, -0.1993543840281266910 ) ) ;
#11852 = COORDINATED_UNIVERSAL_TIME_OFFSET ( 0, 0, .AHEAD. ) ;
#11853 = VECTOR ( 'NONE', #19636, 39.37007874015748143 ) ;
#11854 = CARTESIAN_POINT ( 'NONE',  ( -0.1209015717334110257, 4.047309448929498288, -0.2883025095971109009 ) ) ;
#11855 = CARTESIAN_POINT ( 'NONE',  ( -0.2764156081756484196, 0.1144950937579609918, 0.03625000000000144079 ) ) ;
#11856 = CARTESIAN_POINT ( 'NONE',  ( 0.000000000000000000, 2.740000000000000213, -2.516000000000000014 ) ) ;
#11857 = ORIENTED_EDGE ( 'NONE', *, *, #6925, .T. ) ;
#11858 = CARTESIAN_POINT ( 'NONE',  ( -0.1993543840281267465, 0.4729166665907999501, 0.1993543840281266633 ) ) ;
#11859 = CARTESIAN_POINT ( 'NONE',  ( 0.3119999999999999996, 4.137583333333332725, -0.1292346314604056745 ) ) ;
#11860 = DIRECTION ( 'NONE',  ( -0.000000000000000000, -1.000000000000000000, -0.000000000000000000 ) ) ;
#11861 = CARTESIAN_POINT ( 'NONE',  ( 3.820898013339742174E-17, 5.384999999999999787, 0.3119999999999999996 ) ) ;
#11862 = CARTESIAN_POINT ( 'NONE',  ( 0.1306872919485614071, -0.3155070326520293955, 0.07965277777777936274 ) ) ;
#11863 = ORIENTED_EDGE ( 'NONE', *, *, #20996, .F. ) ;
#11864 = LINE ( 'NONE', #17575, #20407 ) ;
#11865 = EDGE_CURVE ( 'NONE', #14830, #17235, #15682, .T. ) ;
#11866 = CARTESIAN_POINT ( 'NONE',  ( -0.2209708691207961095, 0.2209708691207961373, 0.3869444444444485320 ) ) ;
#11867 = CARTESIAN_POINT ( 'NONE',  ( -0.2819296736111110979, 0.5041666665908000056, -0.1167790944451423396 ) ) ;
#11868 = CARTESIAN_POINT ( 'NONE',  ( -0.2819296736111110424, 0.2263888888130222710, -0.1167790944451423396 ) ) ;
#11869 = ORIENTED_EDGE ( 'NONE', *, *, #22145, .F. ) ;
#11870 = EDGE_CURVE ( 'NONE', #10582, #9441, #13295, .T. ) ;
#11871 = CARTESIAN_POINT ( 'NONE',  ( -0.2819296736111110424, 4.141055555631421470, -0.1167790944451423119 ) ) ;
#11872 = CARTESIAN_POINT ( 'NONE',  ( 0.1236067977499789861, 0.2624999998049151739, -0.3804226065180614236 ) ) ;
#11873 = CARTESIAN_POINT ( 'NONE',  ( 0.2819296736111110979, 4.779944444520310753, 0.1167790944451422425 ) ) ;
#11874 = CARTESIAN_POINT ( 'NONE',  ( 1.910449006669871087E-17, 0.4138888887371559577, -0.3119999999999999996 ) ) ;
#11875 = VERTEX_POINT ( 'NONE', #8387 ) ;
#11876 = CARTESIAN_POINT ( 'NONE',  ( 0.3125000000000000555, -5.740531871003217465E-17, 0.08833333333333501236 ) ) ;
#11877 = CARTESIAN_POINT ( 'NONE',  ( -0.3119999999999999996, 3.835500000151732536, 0.000000000000000000 ) ) ;
#11878 = AXIS2_PLACEMENT_3D ( 'NONE', #8631, #1074, #16076 ) ;
#11879 = EDGE_CURVE ( 'NONE', #17381, #23806, #18177, .T. ) ;
#11880 = CARTESIAN_POINT ( 'NONE',  ( 0.09798969090652687175, -0.2586227216849679156, 0.3880822748423150004 ) ) ;
#11881 =( NAMED_UNIT ( * ) SI_UNIT ( $, .STERADIAN. ) SOLID_ANGLE_UNIT ( ) );
#11882 = ORIENTED_EDGE ( 'NONE', *, *, #13467, .F. ) ;
#11883 = COORDINATED_UNIVERSAL_TIME_OFFSET ( 0, 0, .AHEAD. ) ;
#11884 = ORIENTED_EDGE ( 'NONE', *, *, #14082, .F. ) ;
#11885 = CARTESIAN_POINT ( 'NONE',  ( 2.319244702705235195, 2.291712385858714729, -2.476240473580834323 ) ) ;
#11886 = EDGE_CURVE ( 'NONE', #20229, #1066, #19379, .T. ) ;
#11887 = CARTESIAN_POINT ( 'NONE',  ( -0.2297546890400682940, 5.008753309236311679, 0.2110849256844293531 ) ) ;
#11888 = ORIENTED_EDGE ( 'NONE', *, *, #14253, .F. ) ;
#11889 = CARTESIAN_POINT ( 'NONE',  ( 0.2819296736111110424, 0.1569444443685778234, 0.1167790944451424923 ) ) ;
#11890 = ORIENTED_EDGE ( 'NONE', *, *, #4978, .T. ) ;
#11891 = CARTESIAN_POINT ( 'NONE',  ( 0.2492517591117642817, 4.246397638743545144, 0.1920442392552785815 ) ) ;
#11892 = FACE_OUTER_BOUND ( 'NONE', #22490, .T. ) ;
#11893 = LINE ( 'NONE', #21262, #2743 ) ;
#11894 = VECTOR ( 'NONE', #127, 39.37007874015748854 ) ;
#11895 = CARTESIAN_POINT ( 'NONE',  ( 0.2923287055106771337, 0.3437499999024575814, 0.2123892367102621359 ) ) ;
#11896 = CARTESIAN_POINT ( 'NONE',  ( 0.2330253964033324743, 5.174051372064914389, 0.1822079934528198497 ) ) ;
#11897 = ORIENTED_EDGE ( 'NONE', *, *, #1177, .F. ) ;
#11898 = CARTESIAN_POINT ( 'NONE',  ( 0.3613381517857143232, 0.3651785713310288783, 0.1174058825155741975 ) ) ;
#11899 = CARTESIAN_POINT ( 'NONE',  ( -0.3125000000000000000, 1.913510623667739771E-17, 0.06055555555555702796 ) ) ;
#11900 = CARTESIAN_POINT ( 'NONE',  ( 0.1167790944451424368, 3.981333333409199593, 0.2819296736111110424 ) ) ;
#11901 = CARTESIAN_POINT ( 'NONE',  ( -0.2725502669324379457, -0.3839089073841076560, 0.4290249205313916292 ) ) ;
#11902 = PRODUCT_DEFINITION_FORMATION_WITH_SPECIFIED_SOURCE ( 'ANY', '', #1355, .NOT_KNOWN. ) ;
#11903 = CARTESIAN_POINT ( 'NONE',  ( -0.2911802280149716204, 5.178089509600573237, -0.04337890609128645242 ) ) ;
#11904 = CARTESIAN_POINT ( 'NONE',  ( 0.2206173157302028787, 4.411888889040620931, 0.2206173157302027954 ) ) ;
#11905 = CARTESIAN_POINT ( 'NONE',  ( 0.1167790944451424506, 5.050777777853643791, 0.2819296736111110424 ) ) ;
#11906 = VERTEX_POINT ( 'NONE', #13780 ) ;
#11907 = CARTESIAN_POINT ( 'NONE',  ( -0.2819296736111110979, 3.963972222298087544, 0.000000000000000000 ) ) ;
#11908 = ORIENTED_EDGE ( 'NONE', *, *, #4078, .T. ) ;
#11909 = ORIENTED_EDGE ( 'NONE', *, *, #13812, .F. ) ;
#11910 = APPROVAL_STATUS ( 'not_yet_approved' ) ;
#11911 = EDGE_LOOP ( 'NONE', ( #18052, #9886, #22452, #19000 ) ) ;
#11912 = CARTESIAN_POINT ( 'NONE',  ( 0.000000000000000000, 2.740000000000000213, -2.936000000000001720 ) ) ;
#11913 = DIRECTION ( 'NONE',  ( 0.000000000000000000, 0.000000000000000000, -1.000000000000000000 ) ) ;
#11914 = LOCAL_TIME ( 21, 9, 13.00000000000000000, #10670 ) ;
#11915 = EDGE_LOOP ( 'NONE', ( #10632, #10031, #17963, #7395 ) ) ;
#11916 = CARTESIAN_POINT ( 'NONE',  ( -0.1292346314604058410, 0.04930555540382262208, 0.3119999999999998885 ) ) ;
#11917 = CARTESIAN_POINT ( 'NONE',  ( 0.009944027729119363224, 5.130526759350952481, 0.3066508893901822574 ) ) ;
#11918 = LINE ( 'NONE', #19570, #22027 ) ;
#11919 = CARTESIAN_POINT ( 'NONE',  ( 0.000000000000000000, 5.384999999999999787, -0.3119999999999999996 ) ) ;
#11920 = CARTESIAN_POINT ( 'NONE',  ( -4.638126268221291196E-16, 0.1946428569477723358, -0.4000000000000000222 ) ) ;
#11921 = CARTESIAN_POINT ( 'NONE',  ( 0.1144950937579611444, 0.2764156081756483641, 0.2376388888888919526 ) ) ;
#11922 = CARTESIAN_POINT ( 'NONE',  ( -0.1993543840281267465, 0.1256944443685777957, 0.1993543840281266633 ) ) ;
#11923 = CARTESIAN_POINT ( 'NONE',  ( -0.1954553509668046918, -0.1954553509668046640, -0.1269444444444442766 ) ) ;
#11924 = ORIENTED_EDGE ( 'NONE', *, *, #23996, .T. ) ;
#11925 = CARTESIAN_POINT ( 'NONE',  ( 5.178964085587577574E-17, 4.658416666742532186, 0.2819296736111110979 ) ) ;
#11926 = CARTESIAN_POINT ( 'NONE',  ( 2.977666666666666906, 2.756666666666666821, -0.06666666666666686003 ) ) ;
#11927 = CARTESIAN_POINT ( 'NONE',  ( 5.178964085587577574E-17, 4.588972222298087544, 0.2819296736111110979 ) ) ;
#11928 = LINE ( 'NONE', #2410, #9117 ) ;
#11929 = CARTESIAN_POINT ( 'NONE',  ( 0.3084778088542702301, 4.861392285864870821, 0.06361362161637863777 ) ) ;
#11930 = CARTESIAN_POINT ( 'NONE',  ( 0.07641315408907055351, -6.434570819605719236E-16, 0.3613612515901026834 ) ) ;
#11931 = DIRECTION ( 'NONE',  ( 0.000000000000000000, 1.000000000000000000, 0.000000000000000000 ) ) ;
#11932 = CARTESIAN_POINT ( 'NONE',  ( 0.3119999999999999996, 4.245222222222222008, -3.820898013339742174E-17 ) ) ;
#11933 = DIRECTION ( 'NONE',  ( 1.000000000000000000, 0.000000000000000000, 0.000000000000000000 ) ) ;
#11934 = CARTESIAN_POINT ( 'NONE',  ( -0.3119999999999998885, 5.116750000151732536, 0.1292346314604058410 ) ) ;
#11935 = EDGE_CURVE ( 'NONE', #7491, #16373, #7446, .T. ) ;
#11936 = CARTESIAN_POINT ( 'NONE',  ( 0.06194388087313247582, 4.962233402074594402, 0.3057891118530218222 ) ) ;
#11937 = SECURITY_CLASSIFICATION ( '', '', #23540 ) ;
#11938 = ORIENTED_EDGE ( 'NONE', *, *, #4244, .T. ) ;
#11939 = DIRECTION ( 'NONE',  ( -0.000000000000000000, -1.000000000000000000, -0.000000000000000000 ) ) ;
#11940 = ORIENTED_EDGE ( 'NONE', *, *, #8157, .F. ) ;
#11941 = CARTESIAN_POINT ( 'NONE',  ( 0.2372985009168012693, 4.702956468199077200, -0.2041371284000717268 ) ) ;
#11942 = DESIGN_CONTEXT ( 'detailed design', #7951, 'design' ) ;
#11943 = AXIS2_PLACEMENT_3D ( 'NONE', #11404, #420, #22731 ) ;
#11944 = CARTESIAN_POINT ( 'NONE',  ( 1.201146141948970407E-06, 4.904991752689871198, 0.3119999999951060254 ) ) ;
#11945 = CARTESIAN_POINT ( 'NONE',  ( -0.3155070326520292845, 1.931923388228935888E-17, 0.06576388888889080075 ) ) ;
#11946 = CARTESIAN_POINT ( 'NONE',  ( 0.2774186958558277349, 0.3935988683107602415, 0.07439726544912801665 ) ) ;
#11947 = CARTESIAN_POINT ( 'NONE',  ( -0.1571289607070218142, 3.937354179263907294, -0.2726214474784059982 ) ) ;
#11948 =( BOUNDED_CURVE ( )  B_SPLINE_CURVE ( 2, ( #2748, #20921, #2398, #19334, #9836, #4214, #19449, #6158, #21160 ),
 .UNSPECIFIED., .F., .T. ) 
 B_SPLINE_CURVE_WITH_KNOTS ( ( 3, 2, 2, 2, 3 ),
 ( 0.4791666666666666852, 0.4895833333333333148, 0.5000000000000000000, 0.5104166666666666297, 0.5208333333333333703 ),
 .UNSPECIFIED. ) 
 CURVE ( )  GEOMETRIC_REPRESENTATION_ITEM ( )  RATIONAL_B_SPLINE_CURVE ( ( 1.000000000000000000, 0.9238795325112867385, 1.000000000000000000, 0.9238795325112867385, 1.000000000000000000, 0.9238795325112867385, 1.000000000000000000, 0.9238795325112867385, 1.000000000000000000 ) ) 
 REPRESENTATION_ITEM ( '' )  );
#11949 = SECURITY_CLASSIFICATION ( '', '', #5977 ) ;
#11950 = CARTESIAN_POINT ( 'NONE',  ( -0.3613381517857143232, 0.09732142847388615403, -0.1174058825155741004 ) ) ;
#11951 = DIRECTION ( 'NONE',  ( -0.5000000000000003331, 0.000000000000000000, 0.8660254037844384856 ) ) ;
#11952 = DIRECTION ( 'NONE',  ( -1.224646799147350495E-16, 0.000000000000000000, -1.000000000000000000 ) ) ;
#11953 = CARTESIAN_POINT ( 'NONE',  ( -3.827021247335479543E-17, -0.3125000000000000000, 0.4147222222222268773 ) ) ;
#11954 = DIRECTION ( 'NONE',  ( 0.8660254037844383745, 0.000000000000000000, 0.5000000000000004441 ) ) ;
#11955 = CARTESIAN_POINT ( 'NONE',  ( 1.726321361862525858E-17, 0.6187499999241333759, -0.2819296736111110979 ) ) ;
#11956 = ORIENTED_EDGE ( 'NONE', *, *, #3944, .F. ) ;
#11957 = CARTESIAN_POINT ( 'NONE',  ( -0.1556145064993704752, 5.113981281356894115, 0.2680637230490377498 ) ) ;
#11958 = DIRECTION ( 'NONE',  ( 0.000000000000000000, 1.000000000000000000, 0.000000000000000000 ) ) ;
#11959 = CARTESIAN_POINT ( 'NONE',  ( -0.2209708691207961095, 0.2209708691207961373, 0.3383333333333373716 ) ) ;
#11960 = CARTESIAN_POINT ( 'NONE',  ( -0.1292346314604058410, 0.5562499999999995781, 0.3119999999999998885 ) ) ;
#11961 = CARTESIAN_POINT ( 'NONE',  ( 0.1292346314604056190, 5.033416666666665762, -0.3119999999999999996 ) ) ;
#11962 = VECTOR ( 'NONE', #7542, 39.37007874015748143 ) ;
#11963 = CARTESIAN_POINT ( 'NONE',  ( -0.2819296736111110979, 4.088972222298088433, 0.000000000000000000 ) ) ;
#11964 = CARTESIAN_POINT ( 'NONE',  ( -0.3119999999999999996, 3.828555555555555046, 0.000000000000000000 ) ) ;
#11965 = CARTESIAN_POINT ( 'NONE',  ( -0.1292346314604057300, 3.894527777777776478, 0.3119999999999998885 ) ) ;
#11966 = DIRECTION ( 'NONE',  ( 0.000000000000000000, 0.000000000000000000, -1.000000000000000000 ) ) ;
#11967 = ORIENTED_EDGE ( 'NONE', *, *, #11537, .T. ) ;
#11968 = ORIENTED_EDGE ( 'NONE', *, *, #14854, .F. ) ;
#11969 = DIRECTION ( 'NONE',  ( 0.000000000000000000, 0.000000000000000000, -1.000000000000000000 ) ) ;
#11970 = CARTESIAN_POINT ( 'NONE',  ( 0.1993543840281267465, 4.651472222298087544, 0.1993543840281266633 ) ) ;
#11971 = CARTESIAN_POINT ( 'NONE',  ( 0.1591012008044834503, 0.4494087562524295421, 0.07655254331174679572 ) ) ;
#11972 = CARTESIAN_POINT ( 'NONE',  ( 0.04611292249197068011, -0.5146425691514149303, 0.3901966308178844711 ) ) ;
#11973 = DATE_AND_TIME ( #13683, #2909 ) ;
#11974 = FACE_OUTER_BOUND ( 'NONE', #8127, .T. ) ;
#11975 = ADVANCED_FACE ( 'NONE', ( #4619 ), #23005, .T. ) ;
#11976 = CARTESIAN_POINT ( 'NONE',  ( 0.2764156081756484196, -5.077672346800151106E-17, 0.06055555555555720143 ) ) ;
#11977 = AXIS2_PLACEMENT_3D ( 'NONE', #3924, #11369, #14272 ) ;
#11978 = CARTESIAN_POINT ( 'NONE',  ( -0.1167790944451423119, 4.411888888964754507, -0.2819296736111110979 ) ) ;
#11979 = FACE_OUTER_BOUND ( 'NONE', #1764, .T. ) ;
#11980 = CARTESIAN_POINT ( 'NONE',  ( 0.000000000000000000, 0.2764156081756484196, 0.2480555555555586933 ) ) ;
#11981 = CARTESIAN_POINT ( 'NONE',  ( 0.2977100099089716734, 3.659999999999999698, 0.09499999999999995948 ) ) ;
#11982 = VERTEX_POINT ( 'NONE', #14622 ) ;
#11983 = CARTESIAN_POINT ( 'NONE',  ( 0.2819296736111110424, 0.4347222221463555303, 0.1167790944451424923 ) ) ;
#11984 = CARTESIAN_POINT ( 'NONE',  ( -0.3119999999999999996, 0.1013888888888885564, -3.820898013339742174E-17 ) ) ;
#11985 = CARTESIAN_POINT ( 'NONE',  ( -5.428794840643969700E-10, 4.321611111277808170, -0.3119999999999999996 ) ) ;
#11986 = CARTESIAN_POINT ( 'NONE',  ( 0.4000000000000000222, 0.3999999999999999112, 0.000000000000000000 ) ) ;
#11987 = CARTESIAN_POINT ( 'NONE',  ( 0.3155070326520292845, -5.795770164686806123E-17, 0.1456250000000021139 ) ) ;
#11988 = EDGE_CURVE ( 'NONE', #14521, #12807, #12147, .T. ) ;
#11989 = CARTESIAN_POINT ( 'NONE',  ( 0.1294417382415924134, 0.3124999999999999445, 0.04319444444444578424 ) ) ;
#11990 = CARTESIAN_POINT ( 'NONE',  ( -0.002220744026976864509, 3.766115247783142550, -0.3119932384635896727 ) ) ;
#11991 = CARTESIAN_POINT ( 'NONE',  ( -0.1993543840281266633, 0.5562499999241333759, -0.1993543840281266910 ) ) ;
#11992 = CARTESIAN_POINT ( 'NONE',  ( 0.1993543840281266910, 0.1534722221463555858, -0.1993543840281266910 ) ) ;
#11993 = CARTESIAN_POINT ( 'NONE',  ( 0.2819296736111110979, 4.057722222298088433, 0.1167790944451422425 ) ) ;
#11994 = CARTESIAN_POINT ( 'NONE',  ( 0.1236067977499789028, 0.3053571426620580453, 0.3804226065180614791 ) ) ;
#11995 = CARTESIAN_POINT ( 'NONE',  ( 0.1167790944451424368, 4.606333333409200037, 0.2819296736111110424 ) ) ;
#11996 = CARTESIAN_POINT ( 'NONE',  ( -4.638126268221291196E-16, 0.1946428569477723358, -0.4000000000000000222 ) ) ;
#11997 = VERTEX_POINT ( 'NONE', #19855 ) ;
#11998 = VECTOR ( 'NONE', #7468, 39.37007874015748143 ) ;
#11999 = DIRECTION ( 'NONE',  ( 0.000000000000000000, 0.000000000000000000, -1.000000000000000000 ) ) ;
#12000 = CARTESIAN_POINT ( 'NONE',  ( 0.3119999999999999996, 3.915361111262843252, 0.1292346314604056190 ) ) ;
#12001 = SHAPE_REPRESENTATION ( '94902A107_High-Strength Steel Flange Nut_94902A107', ( #9127 ), #20827 ) ;
#12002 = CARTESIAN_POINT ( 'NONE',  ( -0.1166234456863257940, 1.999640111863030478, -2.617828497045949110 ) ) ;
#12003 = CARTESIAN_POINT ( 'NONE',  ( 0.02897014736687301972, 0.03242967361111054325, 0.2808128927374478612 ) ) ;
#12004 = ADVANCED_FACE ( 'NONE', ( #21922 ), #10720, .T. ) ;
#12005 = CALENDAR_DATE ( 2026, 7, 10 ) ;
#12006 = ORIENTED_EDGE ( 'NONE', *, *, #11260, .T. ) ;
#12007 = CARTESIAN_POINT ( 'NONE',  ( 0.2472135954999579721, 0.3392857142857141350, -0.3402603233408160732 ) ) ;
#12008 = CARTESIAN_POINT ( 'NONE',  ( -0.2890875887038242276, 4.998758336917366485, -0.1173658538989466454 ) ) ;
#12009 = VERTEX_POINT ( 'NONE', #12806 ) ;
#12010 = CARTESIAN_POINT ( 'NONE',  ( -0.1167790944451424368, 0.08749999992413336203, 0.2819296736111110424 ) ) ;
#12011 = AXIS2_PLACEMENT_3D ( 'NONE', #18241, #1540, #14591 ) ;
#12012 = ORIENTED_EDGE ( 'NONE', *, *, #20793, .F. ) ;
#12013 = CARTESIAN_POINT ( 'NONE',  ( -0.06335377612981447915, 0.02316948994475548362, 0.4000000000000000777 ) ) ;
#12014 = CARTESIAN_POINT ( 'NONE',  ( -0.2950224166209188259, 4.727389069448219239, 0.1057762073105751044 ) ) ;
#12015 = CARTESIAN_POINT ( 'NONE',  ( -0.2233192592356399442, 0.3044642856167432132, -0.3073725909049500049 ) ) ;
#12016 = DIRECTION ( 'NONE',  ( 0.000000000000000000, 0.9659258262890680902, 0.2588190451025214611 ) ) ;
#12017 = EDGE_CURVE ( 'NONE', #6354, #16467, #9632, .T. ) ;
#12018 = CARTESIAN_POINT ( 'NONE',  ( 0.3613381517857143232, 0.3687499999024574926, 0.000000000000000000 ) ) ;
#12019 = CARTESIAN_POINT ( 'NONE',  ( -0.4000000000000000222, 0.1410714283763437604, -4.898587196589413075E-17 ) ) ;
#12020 = CARTESIAN_POINT ( 'NONE',  ( -0.1993543840281266355, 3.804250000075865223, 0.1993543840281267465 ) ) ;
#12021 = CARTESIAN_POINT ( 'NONE',  ( -0.1552887038618610549, 5.191068077878869147, 0.2436830441765351074 ) ) ;
#12022 = CARTESIAN_POINT ( 'NONE',  ( 0.000000000000000000, 5.384999999999999787, -0.3119999999999999996 ) ) ;
#12023 = CARTESIAN_POINT ( 'NONE',  ( 0.2206173157302028787, 4.467444444596176290, 0.2206173157302027954 ) ) ;
#12024 = CARTESIAN_POINT ( 'NONE',  ( -0.2819296736111110979, 4.641055555631421470, -0.1167790944451422980 ) ) ;
#12025 = ORIENTED_EDGE ( 'NONE', *, *, #525, .F. ) ;
#12026 = EDGE_CURVE ( 'NONE', #13133, #7381, #23859, .T. ) ;
#12027 = CARTESIAN_POINT ( 'NONE',  ( -0.1167790944451423257, 4.120222222298087544, -0.2819296736111110424 ) ) ;
#12028 = AXIS2_PLACEMENT_3D ( 'NONE', #12517, #10442, #17868 ) ;
#12029 = ORIENTED_EDGE ( 'NONE', *, *, #2235, .T. ) ;
#12030 = CARTESIAN_POINT ( 'NONE',  ( 0.3613381517857143232, 0.2758928570453146878, 0.1174058825155741975 ) ) ;
#12031 = ORIENTED_EDGE ( 'NONE', *, *, #8255, .T. ) ;
#12032 = EDGE_CURVE ( 'NONE', #1184, #7614, #10601, .T. ) ;
#12033 = EDGE_CURVE ( 'NONE', #8220, #3381, #21069, .T. ) ;
#12034 = ORIENTED_EDGE ( 'NONE', *, *, #5219, .T. ) ;
#12035 = APPLICATION_PROTOCOL_DEFINITION ( 'international standard', 'config_control_design', 1994, #9674 ) ;
#12036 = CARTESIAN_POINT ( 'NONE',  ( -0.1334180974147631815, -0.4531173396632154349, 0.4271664148355316382 ) ) ;
#12037 = CARTESIAN_POINT ( 'NONE',  ( 0.1797084794423411680, 3.735609856212664948, -0.2172307604343298448 ) ) ;
#12038 = CARTESIAN_POINT ( 'NONE',  ( 0.2729403726835234467, 5.150705085961851282, -0.1311526151795892881 ) ) ;
#12039 = CARTESIAN_POINT ( 'NONE',  ( -0.4581189881604794678, -0.2644951211353318010, 0.3941886329748525153 ) ) ;
#12040 = CYLINDRICAL_SURFACE ( 'NONE', #6965, 0.4000000000000000222 ) ;
#12041 = EDGE_CURVE ( 'NONE', #21713, #19257, #7181, .T. ) ;
#12042 = LINE ( 'NONE', #15914, #20084 ) ;
#12043 = CARTESIAN_POINT ( 'NONE',  ( -5.178964085587577574E-17, 0.1326388888130222710, 0.2819296736111110979 ) ) ;
#12044 = CARTESIAN_POINT ( 'NONE',  ( -0.1954553509668046918, -0.1954553509668046640, 0.09527777777777970969 ) ) ;
#12045 = EDGE_LOOP ( 'NONE', ( #9108, #2444, #19689, #9208, #7862 ) ) ;
#12046 = CYLINDRICAL_SURFACE ( 'NONE', #1148, 1.243000000000000105 ) ;
#12047 = CARTESIAN_POINT ( 'NONE',  ( -0.2819296736111110979, 4.575083333409199149, 0.000000000000000000 ) ) ;
#12048 = CARTESIAN_POINT ( 'NONE',  ( -0.2799731695447704727, 0.01905728454626067631, -0.06962859169959349781 ) ) ;
#12049 = CARTESIAN_POINT ( 'NONE',  ( -0.1923458283087008946, 0.2387311634213351574, -1.212225631218351030 ) ) ;
#12050 = FACE_OUTER_BOUND ( 'NONE', #6983, .T. ) ;
#12051 = DIRECTION ( 'NONE',  ( 0.000000000000000000, -0.2142211582677922832, 0.9767851838303064360 ) ) ;
#12052 = CARTESIAN_POINT ( 'NONE',  ( 0.1292346314604058410, 4.234805555555554157, 0.3119999999999998885 ) ) ;
#12053 = CARTESIAN_POINT ( 'NONE',  ( 2.356222887430696744, 2.291712385858714729, -2.088288568297006265 ) ) ;
#12054 = CARTESIAN_POINT ( 'NONE',  ( 0.3108937553010620025, 4.973671289738724965, 0.02625051856199436470 ) ) ;
#12055 = CARTESIAN_POINT ( 'NONE',  ( -0.5116234456863466562, 0.9548081934128058723, 2.635972749958888528 ) ) ;
#12056 = ORIENTED_EDGE ( 'NONE', *, *, #15637, .F. ) ;
#12057 = CARTESIAN_POINT ( 'NONE',  ( 0.07200204255845482626, 4.573693138600060770, 0.3053374176464236367 ) ) ;
#12058 = ORIENTED_EDGE ( 'NONE', *, *, #12758, .T. ) ;
#12059 = CARTESIAN_POINT ( 'NONE',  ( -0.3125000000000000000, -0.1294417382415921913, 0.07097222222222411558 ) ) ;
#12060 = VECTOR ( 'NONE', #1923, 39.37007874015748854 ) ;
#12061 = ORIENTED_EDGE ( 'NONE', *, *, #21901, .T. ) ;
#12062 = DIRECTION ( 'NONE',  ( 1.000000000000000000, 0.000000000000000000, 0.000000000000000000 ) ) ;
#12063 = CARTESIAN_POINT ( 'NONE',  ( 0.3155070326520292290, -0.1306872919485616569, 0.1456250000000025580 ) ) ;
#12064 = ADVANCED_FACE ( 'NONE', ( #21689 ), #2157, .F. ) ;
#12065 = CARTESIAN_POINT ( 'NONE',  ( 1.573500000000000343, 2.683750000000000746, -1.412500000000000089 ) ) ;
#12066 = ADVANCED_FACE ( 'NONE', ( #22166 ), #18511, .T. ) ;
#12067 = CARTESIAN_POINT ( 'NONE',  ( -0.2233192592356399442, 0.3044642856167432132, -0.3073725909049500049 ) ) ;
#12068 = CARTESIAN_POINT ( 'NONE',  ( 0.2819296736111110979, 0.1604166665908000333, 0.000000000000000000 ) ) ;
#12069 = CARTESIAN_POINT ( 'NONE',  ( 0.2764156081756483641, 0.1144950937579610056, 0.1265277777777799595 ) ) ;
#12070 = LINE ( 'NONE', #2665, #21700 ) ;
#12071 = CARTESIAN_POINT ( 'NONE',  ( 5.731347020009612645E-17, 5.009111111111110404, 0.3119999999999999996 ) ) ;
#12072 = CARTESIAN_POINT ( 'NONE',  ( -3.385114897866767815E-17, -0.2764156081756484196, 0.4425000000000046119 ) ) ;
#12073 = ORIENTED_EDGE ( 'NONE', *, *, #8264, .F. ) ;
#12074 = CARTESIAN_POINT ( 'NONE',  ( -0.1377698178703422593, 5.114529494886277838, 0.2775902850408615286 ) ) ;
#12075 = CARTESIAN_POINT ( 'NONE',  ( -0.2168203832546517218, 4.272808835557615481, -0.2252774235831185579 ) ) ;
#12076 = CARTESIAN_POINT ( 'NONE',  ( 0.2209708691207961651, 0.2209708691207959985, 0.3244444444444484210 ) ) ;
#12077 = CARTESIAN_POINT ( 'NONE',  ( 0.3119999999999998885, 0.4034722222222218435, 0.1292346314604058410 ) ) ;
#12078 = B_SPLINE_CURVE_WITH_KNOTS ( 'NONE', 3,
 ( #20547, #22367, #18598, #24073, #10682, #23701, #5669, #11170, #18116, #18474, #7382, #10808, #20188, #14833, #22249, #3477, #16533, #5546, #22127, #8966, #18356, #1768, #13011, #20426, #3723, #3355, #7266, #1649, #5428, #11045, #12894, #13134, #18236, #1413, #8841, #14586, #10927, #23952, #7499, #12649, #5307, #12770, #23824, #9083 ),
 .UNSPECIFIED., .F., .F.,
 ( 4, 2, 2, 2, 2, 2, 2, 2, 2, 2, 2, 2, 2, 2, 2, 2, 2, 2, 2, 2, 2, 4 ),
 ( 0.07771480865003008165, 0.07919108110018341362, 0.08066735355033674559, 0.08140548977541341158, 0.08214362600049006369, 0.08361989845064339566, 0.08509617090079674151, 0.08657244335095005960, 0.08731057957602672559, 0.08804871580110339158, 0.08952498825125672355, 0.09026312447633338953, 0.09100126070141005552, 0.09247753315156338749, 0.09395380560171671946, 0.09469194182679338545, 0.09543007805187005144, 0.09690635050202339729, 0.09764448672710004939, 0.09838262295217671538, 0.09985889540233004735, 0.1013351678524833793 ),
 .UNSPECIFIED. ) ;
#12079 = CARTESIAN_POINT ( 'NONE',  ( -0.3119999999999998885, 4.998694444444444329, 0.1292346314604058410 ) ) ;
#12080 = AXIS2_PLACEMENT_3D ( 'NONE', #8333, #2979, #10187 ) ;
#12081 = B_SPLINE_CURVE_WITH_KNOTS ( 'NONE', 3,
 ( #463, #14876, #22414, #5717, #13176, #8015, #2883, #12185, #2657, #15818, #8133, #10222, #21189, #8490, #19591, #15584, #23236, #937, #1062, #15933, #9988, #4478, #4359, #13883, #6187, #823, #8252, #11694, #15467, #19359, #17648, #11815, #17532, #6667, #17770, #10109, #6310, #17412, #15704, #23007 ),
 .UNSPECIFIED., .F., .F.,
 ( 4, 2, 2, 2, 2, 2, 2, 2, 2, 2, 2, 1, 2, 2, 1, 1, 1, 2, 2, 2, 2, 4 ),
 ( 0.7035887612132493141, 0.7060454443609081032, 0.7085021275085668924, 0.7109588106562256815, 0.7121871522300550206, 0.7134154938038844707, 0.7146438353777138097, 0.7158721769515432598, 0.7171005185253725989, 0.7177146893122873239, 0.7180217747057446864, 0.7180409675428357508, 0.7180457657521085446, 0.7180505639613813385, 0.7180601603799268151, 0.7180985460541091658, 0.7181753174024736452, 0.7183288600992028261, 0.7195572016730356069, 0.7207855432468683876, 0.7220138848207011684, 0.7232422263945339491 ),
 .UNSPECIFIED. ) ;
#12082 = CARTESIAN_POINT ( 'NONE',  ( 0.2819296736111110979, 4.061194444520309865, -3.452642723725051716E-17 ) ) ;
#12083 = DIRECTION ( 'NONE',  ( 1.000000000000000000, 0.000000000000000000, 0.000000000000000000 ) ) ;
#12084 = CARTESIAN_POINT ( 'NONE',  ( -0.4212185919419081936, 0.2861805174102238225, 0.4063787963957418148 ) ) ;
#12085 = CARTESIAN_POINT ( 'NONE',  ( 0.1788910854725163091, 4.816197864334125001, -0.2589896416955246305 ) ) ;
#12086 = ORIENTED_EDGE ( 'NONE', *, *, #12442, .T. ) ;
#12087 = ORIENTED_EDGE ( 'NONE', *, *, #21353, .F. ) ;
#12088 = CARTESIAN_POINT ( 'NONE',  ( -0.1571291513240659632, 4.011495724926215978, 0.2726213359419245585 ) ) ;
#12089 = CARTESIAN_POINT ( 'NONE',  ( -0.1993543840281266910, 4.623694444520309865, -0.1993543840281266910 ) ) ;
#12090 = CARTESIAN_POINT ( 'NONE',  ( -0.01469736539579117630, 4.515659913531111513, 0.3117060488516621986 ) ) ;
#12091 = DATE_TIME_ROLE ( 'creation_date' ) ;
#12092 = CARTESIAN_POINT ( 'NONE',  ( -1.889944503261478141E-16, 0.5289902422706634910, 0.3941886329748526263 ) ) ;
#12093 = CC_DESIGN_PERSON_AND_ORGANIZATION_ASSIGNMENT ( #11154, #7485, ( #4493 ) ) ;
#12094 = CIRCLE ( 'NONE', #2771, 0.7500000000000001110 ) ;
#12095 = CARTESIAN_POINT ( 'NONE',  ( -0.2764156081756484196, 1.692557448933383907E-17, 0.03277777777777921009 ) ) ;
#12096 = AXIS2_PLACEMENT_3D ( 'NONE', #21356, #13696, #6473 ) ;
#12097 = CARTESIAN_POINT ( 'NONE',  ( 0.2819296736111110979, 4.009111111186976828, -0.1167790944451423396 ) ) ;
#12098 = COORDINATED_UNIVERSAL_TIME_OFFSET ( 0, 0, .AHEAD. ) ;
#12099 = CARTESIAN_POINT ( 'NONE',  ( -0.2929336088530244964, 4.832415422266893579, -0.1092304483702396245 ) ) ;
#12100 = CARTESIAN_POINT ( 'NONE',  ( 0.01548350045596276134, 5.071997560486030565, 0.3119999982137058314 ) ) ;
#12101 = CARTESIAN_POINT ( 'NONE',  ( 0.2764156081756483641, 0.1144950937579610195, 0.2376388888888919526 ) ) ;
#12102 = CARTESIAN_POINT ( 'NONE',  ( 0.3999999999999999667, 0.2535714285714285032, 0.1299678784931626307 ) ) ;
#12103 = CARTESIAN_POINT ( 'NONE',  ( -0.2819296736111110979, 0.5770833332574666352, -3.452642723725051716E-17 ) ) ;
#12104 = CARTESIAN_POINT ( 'NONE',  ( 0.4795759095149518814, -0.04342522374607015595, 0.07439890854714663326 ) ) ;
#12105 = CARTESIAN_POINT ( 'NONE',  ( 0.000000000000000000, 0.8699999999999998845, -0.2109499999999998043 ) ) ;
#12106 = CARTESIAN_POINT ( 'NONE',  ( 0.2206173157302028787, 4.460499999999998799, 0.2206173157302027954 ) ) ;
#12107 = DIRECTION ( 'NONE',  ( 0.000000000000000000, 0.000000000000000000, 1.000000000000000000 ) ) ;
#12108 = CARTESIAN_POINT ( 'NONE',  ( 0.2230971623002954429, 0.2230971623002953319, 0.4859027777777825685 ) ) ;
#12109 = ORIENTED_EDGE ( 'NONE', *, *, #10509, .F. ) ;
#12110 = CARTESIAN_POINT ( 'NONE',  ( -1.910449006669871087E-17, 3.981333333333332725, -0.3119999999999999996 ) ) ;
#12111 = CARTESIAN_POINT ( 'NONE',  ( 0.1294417382415924134, 0.3124999999999999445, 0.3765277777777817358 ) ) ;
#12112 = CARTESIAN_POINT ( 'NONE',  ( 0.1993543840281266355, 0.4173611110352444808, 0.1993543840281267465 ) ) ;
#12113 = CARTESIAN_POINT ( 'NONE',  ( -0.1993543840281267465, 0.4590277777019111105, 0.1993543840281266633 ) ) ;
#12114 = CARTESIAN_POINT ( 'NONE',  ( -0.2819296736111110979, 4.144527777853643791, 0.000000000000000000 ) ) ;
#12115 = CARTESIAN_POINT ( 'NONE',  ( -0.2923287055106771337, 0.1258928570453147489, 0.2123892367102619971 ) ) ;
#12116 = ORIENTED_EDGE ( 'NONE', *, *, #16978, .T. ) ;
#12117 = CARTESIAN_POINT ( 'NONE',  ( -0.2819296736111110979, 4.700083333409199149, 0.000000000000000000 ) ) ;
#12118 = CYLINDRICAL_SURFACE ( 'NONE', #12391, 0.4000000000000000222 ) ;
#12119 = AXIS2_PLACEMENT_3D ( 'NONE', #11707, #597, #15480 ) ;
#12120 = CARTESIAN_POINT ( 'NONE',  ( 0.2085465366998034975, 5.085798565832035933, -0.2321456212477118752 ) ) ;
#12121 = AXIS2_PLACEMENT_3D ( 'NONE', #13, #1977, #9656 ) ;
#12122 = EDGE_LOOP ( 'NONE', ( #7631, #6452, #22707, #15225 ) ) ;
#12123 = CARTESIAN_POINT ( 'NONE',  ( 1.962866667188212455, 2.690142902515285428, -2.659351702128306183 ) ) ;
#12124 = EDGE_CURVE ( 'NONE', #9581, #14200, #3881, .T. ) ;
#12125 = CARTESIAN_POINT ( 'NONE',  ( -0.1292346314604056745, 3.769527777929509327, -0.3119999999999999996 ) ) ;
#12126 = DIRECTION ( 'NONE',  ( 0.8660254037844382635, 0.000000000000000000, 0.5000000000000007772 ) ) ;
#12127 = ADVANCED_FACE ( 'NONE', ( #22530 ), #9371, .T. ) ;
#12128 = ORIENTED_EDGE ( 'NONE', *, *, #2471, .T. ) ;
#12129 = CARTESIAN_POINT ( 'NONE',  ( 1.910449006669871087E-17, 0.5874999999999996891, -0.3119999999999999996 ) ) ;
#12130 = COORDINATED_UNIVERSAL_TIME_OFFSET ( 0, 0, .AHEAD. ) ;
#12131 = ORIENTED_EDGE ( 'NONE', *, *, #11112, .T. ) ;
#12132 = CARTESIAN_POINT ( 'NONE',  ( -0.2206173157302028787, 0.3236111109593782231, 0.2206173157302027954 ) ) ;
#12133 = DIRECTION ( 'NONE',  ( 0.3535533905932676246, -0.7071067811865477948, 0.6123724356957979120 ) ) ;
#12134 = CARTESIAN_POINT ( 'NONE',  ( 0.1993543840281266910, 0.1673611110352444808, -0.1993543840281266910 ) ) ;
#12135 = AXIS2_PLACEMENT_3D ( 'NONE', #14939, #14579, #1761 ) ;
#12136 = ORIENTED_EDGE ( 'NONE', *, *, #11530, .T. ) ;
#12137 = CARTESIAN_POINT ( 'NONE',  ( -0.1993543840281266633, 0.07013888881302225708, -0.1993543840281266910 ) ) ;
#12138 = CARTESIAN_POINT ( 'NONE',  ( -0.2837606913901806194, 4.720503326065920824, -0.1316857305938944622 ) ) ;
#12139 = CARTESIAN_POINT ( 'NONE',  ( 5.574357792518489764E-07, 4.071633398088104094, 0.3119999999989289674 ) ) ;
#12140 = CARTESIAN_POINT ( 'NONE',  ( 0.3613381517857143232, 0.3508928570453146989, 0.000000000000000000 ) ) ;
#12141 = CARTESIAN_POINT ( 'NONE',  ( -0.2249462833042268628, 5.064501476579637895, 0.2162079342807830262 ) ) ;
#12142 = FACE_OUTER_BOUND ( 'NONE', #10602, .T. ) ;
#12143 = CARTESIAN_POINT ( 'NONE',  ( 1.973001146175420883, 2.291712385858714729, -1.876529041877832205 ) ) ;
#12144 = ORIENTED_EDGE ( 'NONE', *, *, #4085, .F. ) ;
#12145 = CARTESIAN_POINT ( 'NONE',  ( 0.1167790944451422702, 5.238277777853643791, -0.2819296736111110424 ) ) ;
#12146 =( BOUNDED_CURVE ( )  B_SPLINE_CURVE ( 2, ( #22097, #12858, #6866, #12494, #5270, #19914, #14309, #16259, #3321 ),
 .UNSPECIFIED., .F., .T. ) 
 B_SPLINE_CURVE_WITH_KNOTS ( ( 3, 2, 2, 2, 3 ),
 ( 0.6875000000000001110, 0.6919642857142858094, 0.6964285714285713969, 0.7008928571428570953, 0.7053571428571429047 ),
 .UNSPECIFIED. ) 
 CURVE ( )  GEOMETRIC_REPRESENTATION_ITEM ( )  RATIONAL_B_SPLINE_CURVE ( ( 0.9999999999999981126, 0.9238795325112886259, 1.000000000000000000, 0.9238795325112867385, 1.000000000000000000, 0.9238795325112867385, 1.000000000000000000, 0.9238795325112867385, 1.000000000000000000 ) ) 
 REPRESENTATION_ITEM ( '' )  );
#12147 =( BOUNDED_CURVE ( )  B_SPLINE_CURVE ( 2, ( #3268, #22046, #16689, #8752, #5092, #16448, #3152, #16207, #19980 ),
 .UNSPECIFIED., .F., .T. ) 
 B_SPLINE_CURVE_WITH_KNOTS ( ( 3, 2, 2, 2, 3 ),
 ( 0.7291666666666666297, 0.7395833333333333703, 0.7500000000000000000, 0.7604166666666666297, 0.7708333333333333703 ),
 .UNSPECIFIED. ) 
 CURVE ( )  GEOMETRIC_REPRESENTATION_ITEM ( )  RATIONAL_B_SPLINE_CURVE ( ( 1.000000000000000000, 0.9238795325112867385, 1.000000000000000000, 0.9238795325112867385, 1.000000000000000000, 0.9238795325112867385, 1.000000000000000000, 0.9238795325112867385, 1.000000000000000000 ) ) 
 REPRESENTATION_ITEM ( '' )  );
#12148 = CARTESIAN_POINT ( 'NONE',  ( 0.000000000000000000, 5.072999999999999510, 0.000000000000000000 ) ) ;
#12149 = LINE ( 'NONE', #7859, #3128 ) ;
#12150 = CARTESIAN_POINT ( 'NONE',  ( -0.3009862200524689446, 4.777363621821248962, -0.09131534522726025838 ) ) ;
#12151 = CARTESIAN_POINT ( 'NONE',  ( -1.910449006669871087E-17, 4.599388889040620931, -0.3119999999999999996 ) ) ;
#12152 = CARTESIAN_POINT ( 'NONE',  ( 0.2819296736111110979, 4.616750000075865223, -3.452642723725051716E-17 ) ) ;
#12153 = ORIENTED_EDGE ( 'NONE', *, *, #16212, .T. ) ;
#12154 = CARTESIAN_POINT ( 'NONE',  ( 0.2819296736111110979, 3.991750000075865223, -3.452642723725051716E-17 ) ) ;
#12155 = EDGE_LOOP ( 'NONE', ( #23623, #20004, #1872, #17554 ) ) ;
#12156 = ADVANCED_FACE ( 'NONE', ( #13171 ), #14985, .T. ) ;
#12157 = MECHANICAL_CONTEXT ( 'NONE', #9674, 'mechanical' ) ;
#12158 = CARTESIAN_POINT ( 'NONE',  ( 7.478516849590708700E-17, -0.5289902422706634910, 0.3941886329748525153 ) ) ;
#12159 = CARTESIAN_POINT ( 'NONE',  ( 0.5601250000000235207, 0.000000000000000000, -0.05999999999999999084 ) ) ;
#12160 = CARTESIAN_POINT ( 'NONE',  ( -0.1993543840281266910, 3.748694444520310309, -0.1993543840281266910 ) ) ;
#12161 = DIRECTION ( 'NONE',  ( 0.8660254037844526964, 0.000000000000000000, -0.4999999999999757416 ) ) ;
#12162 = CARTESIAN_POINT ( 'NONE',  ( -2.038214714022946347E-16, 0.5196152422706634688, 0.4425000000000000044 ) ) ;
#12163 = CARTESIAN_POINT ( 'NONE',  ( 0.1292346314604043700, 4.644527777777777366, -0.3120000000000012763 ) ) ;
#12164 = CYLINDRICAL_SURFACE ( 'NONE', #18927, 0.2500000000000000000 ) ;
#12165 = CARTESIAN_POINT ( 'NONE',  ( 0.2819296736111110979, 0.1499999999241333482, -0.1167790944451422980 ) ) ;
#12166 = CARTESIAN_POINT ( 'NONE',  ( -0.1954553509668046918, -0.1954553509668046640, 0.03972222222222369925 ) ) ;
#12167 = ORIENTED_EDGE ( 'NONE', *, *, #23884, .T. ) ;
#12168 = DIRECTION ( 'NONE',  ( -0.000000000000000000, -1.000000000000000000, -0.000000000000000000 ) ) ;
#12169 = CARTESIAN_POINT ( 'NONE',  ( 0.1167790944451422702, 4.391055555631420582, -0.2819296736111110424 ) ) ;
#12170 = CARTESIAN_POINT ( 'NONE',  ( 0.02575435819785588942, 0.2888475187005514200, -0.07854616851683961232 ) ) ;
#12171 = CARTESIAN_POINT ( 'NONE',  ( -0.3068635116330460932, 0.5432355565805958575, -1.103811322571780940 ) ) ;
#12172 = CARTESIAN_POINT ( 'NONE',  ( 0.3125000000000000000, -5.740531871003217465E-17, -0.01583333333333210996 ) ) ;
#12173 = CARTESIAN_POINT ( 'NONE',  ( 1.910449006669871087E-17, 0.4694444442927115380, -0.3119999999999999996 ) ) ;
#12174 = CARTESIAN_POINT ( 'NONE',  ( -0.1292346314604056745, 4.373694444444443441, -0.3119999999999999996 ) ) ;
#12175 = EDGE_CURVE ( 'NONE', #10865, #8265, #15720, .T. ) ;
#12176 = CARTESIAN_POINT ( 'NONE',  ( 0.3119999999999999996, 5.141055555707287894, -3.820898013339742174E-17 ) ) ;
#12177 = CARTESIAN_POINT ( 'NONE',  ( 0.3011001227036403383, 4.972027705505035478, 0.08342311245020585242 ) ) ;
#12178 = CARTESIAN_POINT ( 'NONE',  ( 0.4570242136016807732, 0.2774028246161672207, 0.04874733047933993424 ) ) ;
#12179 = ORIENTED_EDGE ( 'NONE', *, *, #5432, .T. ) ;
#12180 = DIRECTION ( 'NONE',  ( -1.000000000000000000, 0.000000000000000000, 0.000000000000000000 ) ) ;
#12181 = VERTEX_POINT ( 'NONE', #14707 ) ;
#12182 = ADVANCED_FACE ( 'NONE', ( #10921 ), #8615, .T. ) ;
#12183 = CARTESIAN_POINT ( 'NONE',  ( 0.000000000000000000, 0.4197679491924312112, 0.000000000000000000 ) ) ;
#12184 =( REPRESENTATION_RELATIONSHIP ('NONE','NONE', #4490, #17931 ) REPRESENTATION_RELATIONSHIP_WITH_TRANSFORMATION ( #18917 )SHAPE_REPRESENTATION_RELATIONSHIP( ) );
#12185 = CARTESIAN_POINT ( 'NONE',  ( 0.2853639214901735333, 4.144740996897934515, -0.1280573243343183787 ) ) ;
#12186 = CARTESIAN_POINT ( 'NONE',  ( -0.1306872919485615459, -0.3155070326520293400, 0.07618055555555755531 ) ) ;
#12187 = FACE_OUTER_BOUND ( 'NONE', #16760, .T. ) ;
#12188 = VECTOR ( 'NONE', #11021, 39.37007874015748854 ) ;
#12189 = DIRECTION ( 'NONE',  ( 0.000000000000000000, 0.000000000000000000, -1.000000000000000000 ) ) ;
#12190 = ADVANCED_FACE ( 'NONE', ( #5420 ), #6659, .F. ) ;
#12191 = CARTESIAN_POINT ( 'NONE',  ( -6.979263641208234666E-17, 0.3330357141881717942, 0.3799334167787516425 ) ) ;
#12192 = CARTESIAN_POINT ( 'NONE',  ( 0.2819296736111110979, 0.05277777770191114520, -0.1167790944451422980 ) ) ;
#12193 = CARTESIAN_POINT ( 'NONE',  ( 0.1954553509668046640, -0.1954553509668047195, 0.06055555555555720143 ) ) ;
#12194 = CARTESIAN_POINT ( 'NONE',  ( 0.3119999999999998885, 0.5145833333333330595, 0.1292346314604058410 ) ) ;
#12195 = CARTESIAN_POINT ( 'NONE',  ( 0.2764156081756484196, -5.077672346800151106E-17, 0.4008333333333376491 ) ) ;
#12196 = ORIENTED_EDGE ( 'NONE', *, *, #12544, .F. ) ;
#12197 = DIRECTION ( 'NONE',  ( 0.000000000000000000, 0.000000000000000000, 1.000000000000000000 ) ) ;
#12198 = CARTESIAN_POINT ( 'NONE',  ( -0.2024076084730564995, 4.272264278896607870, -0.2381172270738897701 ) ) ;
#12199 = DIRECTION ( 'NONE',  ( 0.8660254037844382635, 0.000000000000000000, 0.5000000000000007772 ) ) ;
#12200 = CARTESIAN_POINT ( 'NONE',  ( -0.1292346314604056190, 0.3687499999999996891, -0.3119999999999999996 ) ) ;
#12201 = CARTESIAN_POINT ( 'NONE',  ( 0.1292346314604058410, 4.957027777777776478, 0.3119999999999998885 ) ) ;
#12202 = CARTESIAN_POINT ( 'NONE',  ( 0.1167790944451422702, 4.168833333409199149, -0.2819296736111110979 ) ) ;
#12203 = CARTESIAN_POINT ( 'NONE',  ( -0.2819296736111110979, 4.033416666742532186, 0.000000000000000000 ) ) ;
#12204 = FACE_OUTER_BOUND ( 'NONE', #8918, .T. ) ;
#12205 = CARTESIAN_POINT ( 'NONE',  ( -0.3119999999999999996, 3.884111111111110404, 0.000000000000000000 ) ) ;
#12206 = CARTESIAN_POINT ( 'NONE',  ( 0.3615179832709032870, -1.207678508861138611E-18, 0.002776101469111443704 ) ) ;
#12207 = ORIENTED_EDGE ( 'NONE', *, *, #9829, .T. ) ;
#12208 = CARTESIAN_POINT ( 'NONE',  ( -3.827021247335479543E-17, -0.3125000000000000000, -0.02972222222222110216 ) ) ;
#12209 = CARTESIAN_POINT ( 'NONE',  ( -0.2819296736111110424, 4.411888888964753619, 0.1167790944451424923 ) ) ;
#12210 = AXIS2_PLACEMENT_3D ( 'NONE', #20133, #19890, #7091 ) ;
#12211 = CARTESIAN_POINT ( 'NONE',  ( -0.3119999999999998885, 4.109805555555554157, 0.1292346314604058410 ) ) ;
#12212 = DATE_AND_TIME ( #15495, #11508 ) ;
#12213 = FACE_OUTER_BOUND ( 'NONE', #14942, .T. ) ;
#12214 = CARTESIAN_POINT ( 'NONE',  ( -0.1954553509668046640, 0.1954553509668046918, 0.02583333333333472440 ) ) ;
#12215 = CARTESIAN_POINT ( 'NONE',  ( 0.2819296736111110979, 4.172305555631421470, -3.452642723725051716E-17 ) ) ;
#12216 = CARTESIAN_POINT ( 'NONE',  ( -0.004360456888021747683, 4.821737920469208127, -0.3119738819052217949 ) ) ;
#12217 = CARTESIAN_POINT ( 'NONE',  ( -0.1294417382415922746, -0.3125000000000000000, 0.2931944444444478104 ) ) ;
#12218 = CARTESIAN_POINT ( 'NONE',  ( -0.2764156081756484196, -0.1144950937579609362, 0.2098611111111139405 ) ) ;
#12219 = CARTESIAN_POINT ( 'NONE',  ( 0.2923287055106771337, 0.1473214284738861568, 0.2123892367102621359 ) ) ;
#12220 = CARTESIAN_POINT ( 'NONE',  ( 0.1167790944451423257, 0.04583333325746669074, -0.2819296736111110424 ) ) ;
#12221 = CARTESIAN_POINT ( 'NONE',  ( 0.4687500000000002776, 0.04414013450030943031, 0.09139228974507368486 ) ) ;
#12222 = CARTESIAN_POINT ( 'NONE',  ( 0.3125000000000000000, -5.740531871003217465E-17, 0.3105555555555590819 ) ) ;
#12223 = CARTESIAN_POINT ( 'NONE',  ( -0.3850708708653799439, 0.3189451064140638170, 0.07813342133392807420 ) ) ;
#12224 = DIRECTION ( 'NONE',  ( 0.000000000000000000, 1.000000000000000000, 0.000000000000000000 ) ) ;
#12225 = CARTESIAN_POINT ( 'NONE',  ( 0.1306872919485616846, 0.3155070326520292290, 0.3227083333333368720 ) ) ;
#12226 = CIRCLE ( 'NONE', #15703, 0.2109499999999996100 ) ;
#12227 = CARTESIAN_POINT ( 'NONE',  ( 3.061616997868383018E-17, 0.000000000000000000, -0.2500000000000000000 ) ) ;
#12228 = CARTESIAN_POINT ( 'NONE',  ( -0.2494851997466753513, 3.774217015172883993, -0.1917528079887330095 ) ) ;
#12229 = CARTESIAN_POINT ( 'NONE',  ( -9.626299801968715084E-16, 0.2035714285714284866, -0.4000000000000000222 ) ) ;
#12230 = CARTESIAN_POINT ( 'NONE',  ( 0.1993543840281266910, 0.3756944443685777957, -0.1993543840281266910 ) ) ;
#12231 = CARTESIAN_POINT ( 'NONE',  ( -0.1993543840281266910, 4.082027777853643791, -0.1993543840281266910 ) ) ;
#12232 = CARTESIAN_POINT ( 'NONE',  ( -6.979263641208234666E-17, 0.06517857133102902822, 0.3799334167787516425 ) ) ;
#12233 = VERTEX_POINT ( 'NONE', #18592 ) ;
#12234 = CARTESIAN_POINT ( 'NONE',  ( 0.2819296736111110979, 4.613277777853643791, 0.1167790944451422425 ) ) ;
#12235 = CARTESIAN_POINT ( 'NONE',  ( 0.09881506494190155088, 5.140796054993752584, -0.2887599643961580864 ) ) ;
#12236 = CARTESIAN_POINT ( 'NONE',  ( 2.040570600599760365, 0.000000000000000000, -2.386288568296997870 ) ) ;
#12237 = ORIENTED_EDGE ( 'NONE', *, *, #19144, .T. ) ;
#12238 = DIRECTION ( 'NONE',  ( -0.000000000000000000, -1.000000000000000000, -0.000000000000000000 ) ) ;
#12239 = CARTESIAN_POINT ( 'NONE',  ( -0.2819296736111110424, 5.238277777853643791, -0.1167790944451423119 ) ) ;
#12240 = CARTESIAN_POINT ( 'NONE',  ( 0.4593750000000003664, -0.2760455974562899817, 0.06112444011295372487 ) ) ;
#12241 = VECTOR ( 'NONE', #20032, 39.37007874015748143 ) ;
#12242 = ORIENTED_EDGE ( 'NONE', *, *, #22626, .F. ) ;
#12243 = CARTESIAN_POINT ( 'NONE',  ( 0.2819296736111110979, 4.825083333409199149, -3.452642723725051716E-17 ) ) ;
#12244 = APPROVAL_ROLE ( '' ) ;
#12245 = CARTESIAN_POINT ( 'NONE',  ( -0.2453579118455930796, 5.108600672401633069, -0.1896813902191237244 ) ) ;
#12246 = CARTESIAN_POINT ( 'NONE',  ( 4.589747744727345336E-07, 4.571629220806286753, 0.3119999999992840722 ) ) ;
#12247 = VERTEX_POINT ( 'NONE', #24065 ) ;
#12248 = CARTESIAN_POINT ( 'NONE',  ( 0.2819296736111110979, 0.3270833332574666907, 0.000000000000000000 ) ) ;
#12249 = ORIENTED_EDGE ( 'NONE', *, *, #15547, .T. ) ;
#12250 = CARTESIAN_POINT ( 'NONE',  ( 1.726321361862525858E-17, 0.1187499999241333620, -0.2819296736111110979 ) ) ;
#12251 = CARTESIAN_POINT ( 'NONE',  ( 0.3125000000000000000, 3.864408831653876942E-17, -0.1016666666666665164 ) ) ;
#12252 = DIRECTION ( 'NONE',  ( -0.000000000000000000, -1.000000000000000000, -0.000000000000000000 ) ) ;
#12253 = CARTESIAN_POINT ( 'NONE',  ( -0.3613381517857143232, 0.3151785713310290005, -4.425116109941954795E-17 ) ) ;
#12254 = CARTESIAN_POINT ( 'NONE',  ( -0.01714907257191002066, 5.044294090511437290, -0.3120000000000000551 ) ) ;
#12255 = CARTESIAN_POINT ( 'NONE',  ( 2.055580586463031434, 2.740000000000000213, -2.936000000000001720 ) ) ;
#12256 = CARTESIAN_POINT ( 'NONE',  ( -0.08123984940749030825, 4.657242163357344644, -0.3039884212747680503 ) ) ;
#12257 = CARTESIAN_POINT ( 'NONE',  ( 0.1167790944451424368, 3.814666666742532630, 0.2819296736111110424 ) ) ;
#12258 = CARTESIAN_POINT ( 'NONE',  ( -0.2399726197094832481, 0.04835313003952727146, -0.1767124178163874682 ) ) ;
#12259 = FACE_OUTER_BOUND ( 'NONE', #4116, .T. ) ;
#12260 = CARTESIAN_POINT ( 'NONE',  ( -0.4805070082343983473, -0.2560807851245620048, 0.04413116910602134235 ) ) ;
#12261 = CARTESIAN_POINT ( 'NONE',  ( -0.3071176021544892443, 4.781885710250458388, 0.06789679950010621412 ) ) ;
#12262 = CARTESIAN_POINT ( 'NONE',  ( -1.910449006669871087E-17, 4.488277777929509327, -0.3119999999999999996 ) ) ;
#12263 = CARTESIAN_POINT ( 'NONE',  ( -0.1167790944451423119, 4.800777777853643791, -0.2819296736111110979 ) ) ;
#12264 = ORIENTED_EDGE ( 'NONE', *, *, #17219, .F. ) ;
#12265 = CARTESIAN_POINT ( 'NONE',  ( 0.2819296736111110979, 4.043833333409200037, 0.1167790944451422425 ) ) ;
#12266 = ORIENTED_EDGE ( 'NONE', *, *, #12445, .F. ) ;
#12267 = PRODUCT ( 'Aloris-BXA-Wedge-R', 'Aloris-BXA-Wedge-R', '', ( #11422 ) ) ;
#12268 = EDGE_LOOP ( 'NONE', ( #9275, #20851, #20900 ) ) ;
#12269 = PERSON_AND_ORGANIZATION_ROLE ( 'creator' ) ;
#12270 = VECTOR ( 'NONE', #9073, 39.37007874015748143 ) ;
#12271 = VERTEX_POINT ( 'NONE', #14826 ) ;
#12272 = FACE_OUTER_BOUND ( 'NONE', #7986, .T. ) ;
#12273 = CARTESIAN_POINT ( 'NONE',  ( -0.2209708691207961373, -0.2209708691207961095, 0.2411111111111144123 ) ) ;
#12274 = CARTESIAN_POINT ( 'NONE',  ( 0.3119999999999999996, 0.1256944442927115102, -0.1292346314604056468 ) ) ;
#12275 = CARTESIAN_POINT ( 'NONE',  ( -0.2276520258992634771, 4.384388760381654926, -0.2133517376713266744 ) ) ;
#12276 = EDGE_CURVE ( 'NONE', #10173, #5967, #5542, .T. ) ;
#12277 = DIRECTION ( 'NONE',  ( 0.000000000000000000, 0.000000000000000000, -1.000000000000000000 ) ) ;
#12278 = DIRECTION ( 'NONE',  ( -0.8651979924482662287, 0.04370253788966843578, 0.4995222938423188319 ) ) ;
#12279 =( BOUNDED_CURVE ( )  B_SPLINE_CURVE ( 2, ( #1172, #8610, #4943, #19826, #1051, #1295, #16171, #21528, #21774 ),
 .UNSPECIFIED., .F., .T. ) 
 B_SPLINE_CURVE_WITH_KNOTS ( ( 3, 2, 2, 2, 3 ),
 ( 0.7708333333333333703, 0.7812500000000000000, 0.7916666666666667407, 0.8020833333333334814, 0.8125000000000001110 ),
 .UNSPECIFIED. ) 
 CURVE ( )  GEOMETRIC_REPRESENTATION_ITEM ( )  RATIONAL_B_SPLINE_CURVE ( ( 1.000000000000000000, 0.9238795325112867385, 1.000000000000000000, 0.9238795325112867385, 1.000000000000000000, 0.9238795325112867385, 1.000000000000000000, 0.9238795325112859613, 1.000000000000000888 ) ) 
 REPRESENTATION_ITEM ( '' )  );
#12280 = CC_DESIGN_APPROVAL ( #9095, ( #10901 ) ) ;
#12281 = VERTEX_POINT ( 'NONE', #3470 ) ;
#12282 = DIRECTION ( 'NONE',  ( -0.000000000000000000, -1.000000000000000000, -0.000000000000000000 ) ) ;
#12283 = CARTESIAN_POINT ( 'NONE',  ( 0.000000000000000000, 5.384999999999999787, 0.000000000000000000 ) ) ;
#12284 = CARTESIAN_POINT ( 'NONE',  ( 0.1144950937579609085, -0.2764156081756484751, 0.05013888888889045381 ) ) ;
#12285 = EDGE_CURVE ( 'NONE', #5345, #13418, #10760, .T. ) ;
#12286 = CARTESIAN_POINT ( 'NONE',  ( -0.2819296736111110424, 4.516055555631421470, -0.1167790944451423119 ) ) ;
#12287 = CARTESIAN_POINT ( 'NONE',  ( 0.000000000000000000, 5.384999999999999787, 0.000000000000000000 ) ) ;
#12288 = CARTESIAN_POINT ( 'NONE',  ( -0.3129558008298474192, 0.5134348993187674015, -1.110400460330370542 ) ) ;
#12289 = DIRECTION ( 'NONE',  ( 0.4999999999999901745, 0.000000000000000000, -0.8660254037844443697 ) ) ;
#12290 = DIRECTION ( 'NONE',  ( 0.7071067811865472397, -0.7071067811865476838, -4.229284785449151260E-16 ) ) ;
#12291 = CARTESIAN_POINT ( 'NONE',  ( -0.3119999999999999996, 4.047305555555555046, -0.1292346314604056468 ) ) ;
#12292 = CARTESIAN_POINT ( 'NONE',  ( 5.731347020009612645E-17, 5.064666666666665762, 0.3119999999999999996 ) ) ;
#12293 = CIRCLE ( 'NONE', #14225, 0.4062499999999997780 ) ;
#12294 = CARTESIAN_POINT ( 'NONE',  ( 0.07550810074049957299, 4.962629998519987318, 0.3027891987685060182 ) ) ;
#12295 = ORIENTED_EDGE ( 'NONE', *, *, #209, .T. ) ;
#12296 = LINE ( 'NONE', #21423, #8165 ) ;
#12297 = ORIENTED_EDGE ( 'NONE', *, *, #14696, .T. ) ;
#12298 = LOCAL_TIME ( 21, 9, 13.00000000000000000, #16401 ) ;
#12299 = CARTESIAN_POINT ( 'NONE',  ( -0.5116234456863258950, 4.559812086079793048, -2.813986238491759551 ) ) ;
#12300 = CARTESIAN_POINT ( 'NONE',  ( -0.1306872919485614903, 0.3155070326520293400, -0.05576388888888796774 ) ) ;
#12301 = CARTESIAN_POINT ( 'NONE',  ( 0.3613381517857143232, 0.3723214284738861068, -0.1174058825155740587 ) ) ;
#12302 = EDGE_CURVE ( 'NONE', #5943, #15879, #10415, .T. ) ;
#12303 = CARTESIAN_POINT ( 'NONE',  ( 0.2494962160978485000, 3.813449145089014003, -0.1917383745809272677 ) ) ;
#12304 = CARTESIAN_POINT ( 'NONE',  ( -0.2923287055106771337, 0.2366071427596004584, -0.2123892367102620804 ) ) ;
#12305 = CARTESIAN_POINT ( 'NONE',  ( -1.910449006669871087E-17, 4.814666666666665762, -0.3119999999999999996 ) ) ;
#12306 = CARTESIAN_POINT ( 'NONE',  ( -0.1954553509668046640, 0.1954553509668046918, 0.08833333333333517889 ) ) ;
#12307 = CARTESIAN_POINT ( 'NONE',  ( 0.08808798601665612793, 0.9548081934128058723, 3.071846948291761414 ) ) ;
#12308 = CARTESIAN_POINT ( 'NONE',  ( -0.1167790944451423257, 5.078555555631421470, -0.2819296736111110424 ) ) ;
#12309 = CARTESIAN_POINT ( 'NONE',  ( -0.2764156081756484196, -0.1144950937579609362, 0.3209722222222259891 ) ) ;
#12310 = ADVANCED_FACE ( 'NONE', ( #17838 ), #21733, .T. ) ;
#12311 = ORIENTED_EDGE ( 'NONE', *, *, #5739, .T. ) ;
#12312 = CARTESIAN_POINT ( 'NONE',  ( -0.1360472109712710653, 4.603413381864274179, -0.2814923986826167734 ) ) ;
#12313 = CARTESIAN_POINT ( 'NONE',  ( -0.0003030584613339698703, 4.293824744644136437, 0.3119998912175568351 ) ) ;
#12314 = CC_DESIGN_APPROVAL ( #19391, ( #16981 ) ) ;
#12315 = CARTESIAN_POINT ( 'NONE',  ( -0.4581189881604794678, -0.2644951211353319120, 0.3941886329748524598 ) ) ;
#12316 = CARTESIAN_POINT ( 'NONE',  ( 0.3119999999999999996, 0.4104166666666663188, -0.1292346314604056468 ) ) ;
#12317 = CARTESIAN_POINT ( 'NONE',  ( -0.2206173157302028232, 4.988277777777777366, -0.2206173157302028232 ) ) ;
#12318 = CARTESIAN_POINT ( 'NONE',  ( -1.726321361862525858E-17, 4.172305555631420582, -0.2819296736111110979 ) ) ;
#12319 = CARTESIAN_POINT ( 'NONE',  ( -1.726321361862525858E-17, 3.908416666742532630, -0.2819296736111110979 ) ) ;
#12320 = FACE_OUTER_BOUND ( 'NONE', #10643, .T. ) ;
#12321 = CARTESIAN_POINT ( 'NONE',  ( -0.3858656996965449948, 0.3184862117744308718, 0.4002370417399356284 ) ) ;
#12322 = DIRECTION ( 'NONE',  ( 0.000000000000000000, 0.9961946980917454342, -0.08715574274765830465 ) ) ;
#12323 = ORIENTED_EDGE ( 'NONE', *, *, #21353, .T. ) ;
#12324 = CARTESIAN_POINT ( 'NONE',  ( -0.1294417382415922746, -0.3125000000000000000, -0.03319444444444336062 ) ) ;
#12325 = CARTESIAN_POINT ( 'NONE',  ( -0.1993543840281266910, 4.401472222298088433, -0.1993543840281266910 ) ) ;
#12326 = CARTESIAN_POINT ( 'NONE',  ( -0.3613381517857143232, 0.02589285704531474330, -0.1174058825155741143 ) ) ;
#12327 = CARTESIAN_POINT ( 'NONE',  ( -0.3094355579546126944, 4.501065253622277496, -0.03993151788800097801 ) ) ;
#12328 = PERSON_AND_ORGANIZATION ( #15518, #2538 ) ;
#12329 = DIRECTION ( 'NONE',  ( 0.000000000000000000, 0.000000000000000000, 1.000000000000000000 ) ) ;
#12330 = EDGE_CURVE ( 'NONE', #16668, #6378, #23777, .T. ) ;
#12331 = CARTESIAN_POINT ( 'NONE',  ( -0.1144950937579609918, -0.2764156081756484196, -0.01236111111111004406 ) ) ;
#12332 = LOCAL_TIME ( 21, 9, 13.00000000000000000, #12098 ) ;
#12333 = CARTESIAN_POINT ( 'NONE',  ( 0.1993543840281267465, 4.054250000075865223, 0.1993543840281266633 ) ) ;
#12334 = APPROVAL_STATUS ( 'not_yet_approved' ) ;
#12335 = LINE ( 'NONE', #19509, #6819 ) ;
#12336 = CARTESIAN_POINT ( 'NONE',  ( 0.2658661084243346684, 0.03242967361111057795, 0.09380593400082704036 ) ) ;
#12337 = CARTESIAN_POINT ( 'NONE',  ( 0.1144950937579609085, -0.2764156081756484751, 0.1681944444444469222 ) ) ;
#12338 = CARTESIAN_POINT ( 'NONE',  ( 0.3613381517857143232, -0.05625000009754239222, -0.1174058825155740587 ) ) ;
#12339 = CONICAL_SURFACE ( 'NONE', #2204, 0.2500000000000000555, 0.5235987755985997971 ) ;
#12340 = CARTESIAN_POINT ( 'NONE',  ( 0.2819296736111110424, 0.6013888888130223265, 0.1167790944451424923 ) ) ;
#12341 = CARTESIAN_POINT ( 'NONE',  ( 1.998815303304990465, 2.291712385858714729, -2.661240473580836152 ) ) ;
#12342 = LINE ( 'NONE', #861, #1444 ) ;
#12343 = CARTESIAN_POINT ( 'NONE',  ( -0.2112264183043934263, 0.3573296004273216475, -0.7196412499502125026 ) ) ;
#12344 = CARTESIAN_POINT ( 'NONE',  ( 0.1144950937579609085, -0.2764156081756484751, 0.05013888888889046075 ) ) ;
#12345 = CARTESIAN_POINT ( 'NONE',  ( 0.1306872919485614071, -0.3155070326520293955, 0.3574305555555593594 ) ) ;
#12346 = ORIENTED_EDGE ( 'NONE', *, *, #19305, .F. ) ;
#12347 = CARTESIAN_POINT ( 'NONE',  ( 0.000000000000000000, 5.384999999999999787, -0.3119999999999999996 ) ) ;
#12348 = CARTESIAN_POINT ( 'NONE',  ( 0.1167790944451423535, 0.4694444443685777957, 0.2819296736111110424 ) ) ;
#12349 = CARTESIAN_POINT ( 'NONE',  ( 0.1167790944451424368, 3.995222222298087988, 0.2819296736111110424 ) ) ;
#12350 = CARTESIAN_POINT ( 'NONE',  ( -0.1116596296178199582, -0.03839285724039952913, -0.3436530038418508792 ) ) ;
#12351 = ORIENTED_EDGE ( 'NONE', *, *, #6308, .F. ) ;
#12352 = CARTESIAN_POINT ( 'NONE',  ( -0.1167790944451423535, 4.599388888964754507, 0.2819296736111110424 ) ) ;
#12353 = CARTESIAN_POINT ( 'NONE',  ( 0.1533627255593470462, 5.139211491064951787, -0.2637066568091733787 ) ) ;
#12354 = DIRECTION ( 'NONE',  ( -0.000000000000000000, -1.000000000000000000, -0.000000000000000000 ) ) ;
#12355 = ORIENTED_EDGE ( 'NONE', *, *, #2715, .F. ) ;
#12356 = CARTESIAN_POINT ( 'NONE',  ( 0.2206173157302027954, 4.029944444444443441, -0.2206173157302028232 ) ) ;
#12357 = CARTESIAN_POINT ( 'NONE',  ( 0.2819296736111110979, 5.213972222298088433, -3.452642723725051716E-17 ) ) ;
#12358 = CARTESIAN_POINT ( 'NONE',  ( 0.2650429728237971294, 4.191665852671973447, 0.1646101441917078023 ) ) ;
#12359 = CIRCLE ( 'NONE', #23232, 0.001000000000000037101 ) ;
#12360 = CARTESIAN_POINT ( 'NONE',  ( 0.1386474987925107871, 0.03242967361111057795, 0.2459144974368996650 ) ) ;
#12361 = CARTESIAN_POINT ( 'NONE',  ( 0.01738314693924293206, 5.206640035683670398, 0.2819296736111598367 ) ) ;
#12362 = CARTESIAN_POINT ( 'NONE',  ( -0.1993543840281266910, 4.957027777853642903, -0.1993543840281266910 ) ) ;
#12363 = PERSON_AND_ORGANIZATION ( #15518, #2538 ) ;
#12364 = ORIENTED_EDGE ( 'NONE', *, *, #17117, .T. ) ;
#12365 = CARTESIAN_POINT ( 'NONE',  ( -0.2934150973083375913, 5.117997740190176614, 0.09815118981130775688 ) ) ;
#12366 = DIRECTION ( 'NONE',  ( 0.000000000000000000, -1.000000000000000000, 0.000000000000000000 ) ) ;
#12367 = ORIENTED_EDGE ( 'NONE', *, *, #7039, .F. ) ;
#12368 = CARTESIAN_POINT ( 'NONE',  ( -0.2819296736111110424, 0.4069444443685779067, -0.1167790944451423396 ) ) ;
#12369 = DIRECTION ( 'NONE',  ( -0.000000000000000000, -1.000000000000000000, -0.000000000000000000 ) ) ;
#12370 = ADVANCED_FACE ( 'NONE', ( #4663 ), #8799, .T. ) ;
#12371 = DIRECTION ( 'NONE',  ( 0.7071067811865484609, 8.659560562354943952E-17, -0.7071067811865464625 ) ) ;
#12372 = DIRECTION ( 'NONE',  ( 0.7071067811865475727, -0.7071067811865475727, 0.000000000000000000 ) ) ;
#12373 = CARTESIAN_POINT ( 'NONE',  ( 0.3613381517857143232, 0.2830357141881717498, -0.1174058825155740587 ) ) ;
#12374 = CARTESIAN_POINT ( 'NONE',  ( -0.2301007481662196430, 5.064294881705610152, 0.2107077067205023468 ) ) ;
#12375 = ADVANCED_FACE ( 'NONE', ( #1371 ), #14423, .T. ) ;
#12376 = CARTESIAN_POINT ( 'NONE',  ( 5.731347020009612645E-17, 3.786888888888888527, 0.3119999999999999996 ) ) ;
#12377 = DIRECTION ( 'NONE',  ( 0.000000000000000000, 0.000000000000000000, 1.000000000000000000 ) ) ;
#12378 = CARTESIAN_POINT ( 'NONE',  ( 0.1167790944451422702, 4.627166666742533074, -0.2819296736111110424 ) ) ;
#12379 = VECTOR ( 'NONE', #23197, 39.37007874015748854 ) ;
#12380 = EDGE_LOOP ( 'NONE', ( #997, #231, #11632, #23290 ) ) ;
#12381 = DIRECTION ( 'NONE',  ( -1.000000000000000000, 0.000000000000000000, 0.000000000000000000 ) ) ;
#12382 = CARTESIAN_POINT ( 'NONE',  ( -0.1167790944451423535, 3.752166666742532630, 0.2819296736111110424 ) ) ;
#12383 = CARTESIAN_POINT ( 'NONE',  ( -0.1844930076592919965, 0.04690905832487239635, -0.2328264863501848803 ) ) ;
#12384 = CARTESIAN_POINT ( 'NONE',  ( 0.03899446768531367874, 5.017119825889835738, 0.3095914530902155737 ) ) ;
#12385 = CARTESIAN_POINT ( 'NONE',  ( -0.4687500000000022760, -0.2630304559196449121, 0.05971082423031025266 ) ) ;
#12386 = CARTESIAN_POINT ( 'NONE',  ( -0.03821043196831897665, 4.792783218731831774, 0.3097114644149256968 ) ) ;
#12387 = CARTESIAN_POINT ( 'NONE',  ( 0.3119999999999999996, 4.193138889040620931, 0.1292346314604056190 ) ) ;
#12388 = CARTESIAN_POINT ( 'NONE',  ( 0.1993543840281267465, 4.665361111186976828, 0.1993543840281266633 ) ) ;
#12389 = CARTESIAN_POINT ( 'NONE',  ( 5.178964085587577574E-17, 4.033416666742532186, 0.2819296736111110979 ) ) ;
#12390 = VERTEX_POINT ( 'NONE', #5137 ) ;
#12391 = AXIS2_PLACEMENT_3D ( 'NONE', #8916, #23528, #14285 ) ;
#12392 = VERTEX_POINT ( 'NONE', #12602 ) ;
#12393 = CALENDAR_DATE ( 2026, 7, 10 ) ;
#12394 = PRODUCT_RELATED_PRODUCT_CATEGORY ( 'detail', '', ( #19646 ) ) ;
#12395 = CARTESIAN_POINT ( 'NONE',  ( 0.000000000000000000, 0.1799999999999999933, 0.000000000000000000 ) ) ;
#12396 = PLANE ( 'NONE',  #3436 ) ;
#12397 = EDGE_LOOP ( 'NONE', ( #13784, #17263, #576, #1035 ) ) ;
#12398 = CARTESIAN_POINT ( 'NONE',  ( -0.3119999999999999996, 0.3687499998482670627, -0.1292346314604056745 ) ) ;
#12399 = CARTESIAN_POINT ( 'NONE',  ( -0.04075253542306750409, 4.403731456933130950, 0.3120000054653133126 ) ) ;
#12400 = CARTESIAN_POINT ( 'NONE',  ( -0.4593752539607652285, 0.04502204785529886899, 0.4343880498115386124 ) ) ;
#12401 = CARTESIAN_POINT ( 'NONE',  ( -9.626299801968715084E-16, 0.3464285714285713635, -0.4000000000000000222 ) ) ;
#12402 = VERTEX_POINT ( 'NONE', #23186 ) ;
#12403 = DIRECTION ( 'NONE',  ( 0.000000000000000000, 0.000000000000000000, -1.000000000000000000 ) ) ;
#12404 = CARTESIAN_POINT ( 'NONE',  ( 1.726321361862525858E-17, 0.6187499999241333759, -0.2819296736111110979 ) ) ;
#12405 = CARTESIAN_POINT ( 'NONE',  ( -0.1144950937579609918, -0.2764156081756484196, 0.09875000000000196121 ) ) ;
#12406 = CARTESIAN_POINT ( 'NONE',  ( -0.2819296736111110424, 4.460500000075867000, -0.1167790944451423119 ) ) ;
#12407 = CARTESIAN_POINT ( 'NONE',  ( 0.1347750699935957031, 0.2587654721081569797, -0.08077297511795365759 ) ) ;
#12408 = CARTESIAN_POINT ( 'NONE',  ( -0.2371691208608801282, 0.6790887934624100231, -1.083708510387177082 ) ) ;
#12409 = CARTESIAN_POINT ( 'NONE',  ( 0.4749999999999999778, 3.575000000000000622, 2.908536147974959276E-17 ) ) ;
#12410 = DIRECTION ( 'NONE',  ( -0.8635502596144366549, -0.07555085810113186529, -0.4985709748471343072 ) ) ;
#12411 = CARTESIAN_POINT ( 'NONE',  ( 5.731347020009612645E-17, 4.064666666666665762, 0.3119999999999999996 ) ) ;
#12412 = AXIS2_PLACEMENT_3D ( 'NONE', #12760, #11157, #16759 ) ;
#12413 = CARTESIAN_POINT ( 'NONE',  ( 0.3119999999999999996, 4.977861111262843252, -0.1292346314604056745 ) ) ;
#12414 = CARTESIAN_POINT ( 'NONE',  ( -1.910449006669871087E-17, 4.870222222222222008, -0.3119999999999999996 ) ) ;
#12415 = EDGE_LOOP ( 'NONE', ( #5509, #23686, #5453, #4064 ) ) ;
#12416 = CARTESIAN_POINT ( 'NONE',  ( 0.04357916212451937166, 5.199516353566889570, 0.2819848337134137628 ) ) ;
#12417 = CARTESIAN_POINT ( 'NONE',  ( -0.1904734272879128332, 4.883006184772527902, -0.2471112552497352621 ) ) ;
#12418 = ADVANCED_FACE ( 'NONE', ( #6495 ), #4635, .F. ) ;
#12419 = CARTESIAN_POINT ( 'NONE',  ( -3.863846776457871776E-17, -0.3155070326520292845, -0.03145833333333220710 ) ) ;
#12420 = CARTESIAN_POINT ( 'NONE',  ( -0.1993543840281266910, 5.234805555631421470, -0.1993543840281266910 ) ) ;
#12421 =( BOUNDED_CURVE ( )  B_SPLINE_CURVE ( 2, ( #12401, #8714, #8837, #14335, #1165, #10563, #3352, #16286, #1409, #10679, #18234, #21767, #8964 ),
 .UNSPECIFIED., .F., .F. ) 
 B_SPLINE_CURVE_WITH_KNOTS ( ( 3, 2, 2, 2, 2, 2, 3 ),
 ( 0.8928571428571429047, 0.9000000000000000222, 0.9142857142857142572, 0.9285714285714286031, 0.9428571428571428381, 0.9571428571428571841, 0.9642857142857143016 ),
 .UNSPECIFIED. ) 
 CURVE ( )  GEOMETRIC_REPRESENTATION_ITEM ( )  RATIONAL_B_SPLINE_CURVE ( ( 0.9755282581475768211, 0.9755282581475769321, 1.000000000000000000, 0.9510565162951535312, 1.000000000000000000, 0.9510565162951535312, 1.000000000000000000, 0.9510565162951535312, 1.000000000000000000, 0.9510565162951535312, 1.000000000000000000, 0.9755282581475768211, 0.9755282581475768211 ) ) 
 REPRESENTATION_ITEM ( '' )  );
#12422 = VECTOR ( 'NONE', #18949, 39.37007874015748143 ) ;
#12423 = CARTESIAN_POINT ( 'NONE',  ( 0.2494960010015663254, 3.801995302344789440, 0.1917386440423899940 ) ) ;
#12424 = ORIENTED_EDGE ( 'NONE', *, *, #6488, .T. ) ;
#12425 = CARTESIAN_POINT ( 'NONE',  ( -0.2233192592356399997, 0.2544642856167432243, 0.3073725909049499494 ) ) ;
#12426 = CARTESIAN_POINT ( 'NONE',  ( -0.2819296736111111534, 0.1361111110352444808, 0.1167790944451422563 ) ) ;
#12427 = CARTESIAN_POINT ( 'NONE',  ( 0.1144950937579609085, -0.2764156081756484751, 0.05708333333333493603 ) ) ;
#12428 = CARTESIAN_POINT ( 'NONE',  ( 0.3613381517857143232, 0.2294642856167432854, -0.1174058825155740587 ) ) ;
#12429 = CARTESIAN_POINT ( 'NONE',  ( -0.1993543840281266355, 5.207027777853642903, 0.1993543840281267465 ) ) ;
#12430 = CARTESIAN_POINT ( 'NONE',  ( 0.1954553509668046640, -0.1954553509668047195, 0.3938888888888931739 ) ) ;
#12431 = LINE ( 'NONE', #1560, #23896 ) ;
#12432 = CARTESIAN_POINT ( 'NONE',  ( -0.2968342663916302970, 4.282823203675612866, 0.1006737699901302241 ) ) ;
#12433 = DIRECTION ( 'NONE',  ( -0.000000000000000000, -1.000000000000000000, -0.000000000000000000 ) ) ;
#12434 = CARTESIAN_POINT ( 'NONE',  ( -0.2206173157302027954, 0.5388888888888885287, -0.2206173157302028232 ) ) ;
#12435 = CARTESIAN_POINT ( 'NONE',  ( -0.1292346314604057023, 4.727861111111110404, 0.3119999999999998885 ) ) ;
#12436 = CARTESIAN_POINT ( 'NONE',  ( 5.178964085587577574E-17, 4.200083333409199149, 0.2819296736111110979 ) ) ;
#12437 = DIRECTION ( 'NONE',  ( 1.000000000000000000, -0.000000000000000000, 0.000000000000000000 ) ) ;
#12438 = CARTESIAN_POINT ( 'NONE',  ( 1.020000000000000018, 2.665000000000000036, -2.591000000000000192 ) ) ;
#12439 = DIRECTION ( 'NONE',  ( 0.4999999999999942268, 0.000000000000000000, -0.8660254037844420383 ) ) ;
#12440 = VECTOR ( 'NONE', #19715, 39.37007874015748854 ) ;
#12441 = CARTESIAN_POINT ( 'NONE',  ( 0.2209708691207961651, 0.2209708691207959985, 0.1022222222222243793 ) ) ;
#12442 = EDGE_CURVE ( 'NONE', #17107, #20052, #3799, .T. ) ;
#12443 = CARTESIAN_POINT ( 'NONE',  ( -1.726321361862525858E-17, 4.561194444520309865, -0.2819296736111110979 ) ) ;
#12444 = CARTESIAN_POINT ( 'NONE',  ( 0.2977100099089716734, 3.659999999999999698, -0.09499999999999995948 ) ) ;
#12445 = EDGE_CURVE ( 'NONE', #3821, #17621, #11243, .T. ) ;
#12446 = PERSON_AND_ORGANIZATION ( #15518, #2538 ) ;
#12447 = CARTESIAN_POINT ( 'NONE',  ( -0.4500000000000003997, -0.2598076211353319009, 0.4425000000000000044 ) ) ;
#12448 = CARTESIAN_POINT ( 'NONE',  ( 0.1144950937579611444, 0.2764156081756483641, 0.01541666666666797678 ) ) ;
#12449 = CARTESIAN_POINT ( 'NONE',  ( 0.2819296736111110979, 4.116750000075866112, -3.452642723725051716E-17 ) ) ;
#12450 = CARTESIAN_POINT ( 'NONE',  ( -0.3061149493775596753, 4.833804916956971454, -0.06113088645964446372 ) ) ;
#12451 = DIRECTION ( 'NONE',  ( 0.8660254037844434816, 0.000000000000000000, -0.4999999999999913403 ) ) ;
#12452 = CARTESIAN_POINT ( 'NONE',  ( -3.385114897866767815E-17, -0.2764156081756484196, 0.1091666666666686880 ) ) ;
#12453 = CARTESIAN_POINT ( 'NONE',  ( 0.3613381517857143232, 0.008035714188171885417, 0.1174058825155742114 ) ) ;
#12454 = CARTESIAN_POINT ( 'NONE',  ( 0.2819296736111110979, 0.6048611110352444253, 0.000000000000000000 ) ) ;
#12455 = CARTESIAN_POINT ( 'NONE',  ( -0.1261236974911686404, 0.2628820852880375813, 0.4030844371307044094 ) ) ;
#12456 = LINE ( 'NONE', #10263, #19730 ) ;
#12457 = DIRECTION ( 'NONE',  ( -1.000000000000000000, 0.000000000000000000, 0.000000000000000000 ) ) ;
#12458 = CARTESIAN_POINT ( 'NONE',  ( -0.01833836887209681216, -0.2764156081756484751, -0.06500058086764817777 ) ) ;
#12459 = CARTESIAN_POINT ( 'NONE',  ( -0.3155070326520293400, -0.1306872919485614626, 0.3990972222222263777 ) ) ;
#12460 = ORIENTED_EDGE ( 'NONE', *, *, #5743, .F. ) ;
#12461 = CARTESIAN_POINT ( 'NONE',  ( 0.4687500000000002220, 0.2630787017013384577, 0.3892820121258428467 ) ) ;
#12462 = CARTESIAN_POINT ( 'NONE',  ( -0.1167790944451424368, 0.4624999999241333759, 0.2819296736111110424 ) ) ;
#12463 = CARTESIAN_POINT ( 'NONE',  ( 0.2819296736111110979, 3.835500000075866556, 0.1167790944451422425 ) ) ;
#12464 = CARTESIAN_POINT ( 'NONE',  ( -0.2233192592356399997, 0.05803571418817188299, 0.3073725909049499494 ) ) ;
#12465 = ORIENTED_EDGE ( 'NONE', *, *, #22587, .T. ) ;
#12466 = CARTESIAN_POINT ( 'NONE',  ( 0.2819296736111110424, 4.564666666742532186, -0.1167790944451423396 ) ) ;
#12467 = CARTESIAN_POINT ( 'NONE',  ( 0.3045549119083980627, 5.129919930104686721, 0.04183624683181733084 ) ) ;
#12468 = ADVANCED_FACE ( 'NONE', ( #13090 ), #16846, .F. ) ;
#12469 = CARTESIAN_POINT ( 'NONE',  ( -0.1292346314604069513, 4.616749999999999687, 0.3119999999999986673 ) ) ;
#12470 = ADVANCED_FACE ( 'NONE', ( #9164 ), #133, .T. ) ;
#12471 = EDGE_LOOP ( 'NONE', ( #18128, #20415, #8950, #21868 ) ) ;
#12472 = EDGE_CURVE ( 'NONE', #4536, #6549, #5077, .T. ) ;
#12473 = CARTESIAN_POINT ( 'NONE',  ( 0.2206173157302028787, 4.016055555555555046, 0.2206173157302027954 ) ) ;
#12474 = CARTESIAN_POINT ( 'NONE',  ( 5.178964085587577574E-17, 5.200083333409199149, 0.2819296736111110979 ) ) ;
#12475 = CARTESIAN_POINT ( 'NONE',  ( 0.2621946814482496446, 4.191512508530529146, 0.1691344502069037914 ) ) ;
#12476 = VECTOR ( 'NONE', #11296, 39.37007874015748143 ) ;
#12477 = EDGE_CURVE ( 'NONE', #12402, #20545, #7144, .T. ) ;
#12478 =( CONVERSION_BASED_UNIT ( 'INCH', #21729 ) LENGTH_UNIT ( ) NAMED_UNIT ( #15699 ) );
#12479 = CARTESIAN_POINT ( 'NONE',  ( 0.06335377612981404893, 0.2642409183210992496, -0.4000000000000001887 ) ) ;
#12480 = CARTESIAN_POINT ( 'NONE',  ( 0.2819296736111110979, 4.884111111186975940, -0.1167790944451423396 ) ) ;
#12481 = APPROVAL_DATE_TIME ( #11121, #5231 ) ;
#12482 = VERTEX_POINT ( 'NONE', #12968 ) ;
#12483 = CARTESIAN_POINT ( 'NONE',  ( -0.3119999999999999996, 0.3131944442927115380, -0.1292346314604056745 ) ) ;
#12484 = CARTESIAN_POINT ( 'NONE',  ( -0.3102354826482426331, 4.556271949145164868, -0.05181833945654303747 ) ) ;
#12485 = ORIENTED_EDGE ( 'NONE', *, *, #20194, .F. ) ;
#12486 = CARTESIAN_POINT ( 'NONE',  ( 1.726321361862525858E-17, 0.2854166665908000056, -0.2819296736111110979 ) ) ;
#12487 = ORIENTED_EDGE ( 'NONE', *, *, #20646, .T. ) ;
#12488 = LINE ( 'NONE', #10644, #15195 ) ;
#12489 = LINE ( 'NONE', #4909, #12725 ) ;
#12490 = CARTESIAN_POINT ( 'NONE',  ( -0.5116234456863466562, 3.514980167629567998, 2.549370209580444691 ) ) ;
#12491 = CARTESIAN_POINT ( 'NONE',  ( 2.575339694675500462E-17, -0.08214285714285715634, -0.4205848896953069405 ) ) ;
#12492 = CARTESIAN_POINT ( 'NONE',  ( -0.1422641812239349990, 5.047914731991645532, -0.2787100512567418087 ) ) ;
#12493 = EDGE_CURVE ( 'NONE', #14703, #13879, #22108, .T. ) ;
#12494 = CARTESIAN_POINT ( 'NONE',  ( 0.3119999999999999996, 4.193138888888888083, -0.1292346314604056745 ) ) ;
#12495 = AXIS2_PLACEMENT_3D ( 'NONE', #12283, #3001, #8350 ) ;
#12496 = CARTESIAN_POINT ( 'NONE',  ( -0.1385637893017130362, 3.881186881039875303, -0.2801137187350042357 ) ) ;
#12497 = DIRECTION ( 'NONE',  ( 0.000000000000000000, 0.000000000000000000, -1.000000000000000000 ) ) ;
#12498 = VECTOR ( 'NONE', #11010, 39.37007874015748854 ) ;
#12499 = CARTESIAN_POINT ( 'NONE',  ( -0.1167790944451423535, 4.710500000075865223, 0.2819296736111110424 ) ) ;
#12500 = CARTESIAN_POINT ( 'NONE',  ( -1.910449006669871087E-17, 4.759111111111110404, -0.3119999999999999996 ) ) ;
#12501 = CARTESIAN_POINT ( 'NONE',  ( -0.1993543840281266355, 3.859805555631421026, 0.1993543840281267465 ) ) ;
#12502 = CARTESIAN_POINT ( 'NONE',  ( -0.2458244892731747677, 0.04853829241537972738, -0.1688004682141546475 ) ) ;
#12503 = CARTESIAN_POINT ( 'NONE',  ( 0.2792459877652407330, 5.034052277606470227, -0.1393239653528951794 ) ) ;
#12504 = CARTESIAN_POINT ( 'NONE',  ( -0.4621664414996935477, -0.2744339579550151287, 0.05971062996526614597 ) ) ;
#12505 = CARTESIAN_POINT ( 'NONE',  ( -0.01780161371572347787, 4.793364628393688598, 0.3116243167563513272 ) ) ;
#12506 = CARTESIAN_POINT ( 'NONE',  ( 0.3119999999999999996, 4.366750000151731648, -0.1292346314604056745 ) ) ;
#12507 = CARTESIAN_POINT ( 'NONE',  ( 0.2819296736111110979, 4.672305555631421470, -3.452642723725051716E-17 ) ) ;
#12508 = CARTESIAN_POINT ( 'NONE',  ( 0.1993543840281267465, 3.873694444520310309, 0.1993543840281266633 ) ) ;
#12509 = VERTEX_POINT ( 'NONE', #11364 ) ;
#12510 = EDGE_CURVE ( 'NONE', #8566, #4354, #2300, .T. ) ;
#12511 = EDGE_CURVE ( 'NONE', #20369, #18391, #18726, .T. ) ;
#12512 = EDGE_LOOP ( 'NONE', ( #7747, #17349, #11499, #12061 ) ) ;
#12513 = VECTOR ( 'NONE', #23755, 39.37007874015748143 ) ;
#12514 = AXIS2_PLACEMENT_3D ( 'NONE', #15882, #14060, #21609 ) ;
#12515 = MECHANICAL_CONTEXT ( 'NONE', #13114, 'mechanical' ) ;
#12516 = CARTESIAN_POINT ( 'NONE',  ( -0.04088287987717395544, 4.933903511193491909, -0.3119999993762155310 ) ) ;
#12517 = CARTESIAN_POINT ( 'NONE',  ( -0.6211549996190571798, 0.000000000000000000, -0.1012499999999999928 ) ) ;
#12518 = VERTEX_POINT ( 'NONE', #7817 ) ;
#12519 = CARTESIAN_POINT ( 'NONE',  ( -0.1292346314604056190, 0.2506944442927114824, -0.3119999999999999996 ) ) ;
#12520 = CARTESIAN_POINT ( 'NONE',  ( -0.2236462712880645243, 4.384219027667765722, -0.2175689465940933709 ) ) ;
#12521 = CARTESIAN_POINT ( 'NONE',  ( 1.145733547534701715E-12, 5.130222168000691418, 0.3067077167097377322 ) ) ;
#12522 = CARTESIAN_POINT ( 'NONE',  ( -0.3119999999999999996, 0.2680555555555552139, -3.820898013339742174E-17 ) ) ;
#12523 = CARTESIAN_POINT ( 'NONE',  ( 0.1821285033488274085, 0.4790585882761230763, -0.7275905587198648883 ) ) ;
#12524 = ORIENTED_EDGE ( 'NONE', *, *, #20063, .F. ) ;
#12525 = ORIENTED_EDGE ( 'NONE', *, *, #2142, .F. ) ;
#12526 = CARTESIAN_POINT ( 'NONE',  ( 0.1292346314604057300, 0.2229166665149337201, 0.3119999999999998885 ) ) ;
#12527 = CARTESIAN_POINT ( 'NONE',  ( 0.2819296736111110979, 0.3722222221463555858, -0.1167790944451422980 ) ) ;
#12528 = CARTESIAN_POINT ( 'NONE',  ( -0.2764156081756484196, 1.692557448933383907E-17, 0.3661111111111152172 ) ) ;
#12529 = CARTESIAN_POINT ( 'NONE',  ( -0.1993543840281266910, 4.345916666742532186, -0.1993543840281266910 ) ) ;
#12530 = CARTESIAN_POINT ( 'NONE',  ( 0.2206173157302027676, 0.1777777777777774515, 0.2206173157302028787 ) ) ;
#12531 = CARTESIAN_POINT ( 'NONE',  ( 0.3860879860166477329, 3.066692553488282957, 2.740461747820544414 ) ) ;
#12532 = CARTESIAN_POINT ( 'NONE',  ( -0.05138680331271978929, 4.236846235768294555, 0.3078081964070191745 ) ) ;
#12533 = CARTESIAN_POINT ( 'NONE',  ( -0.3119999999999999996, 4.102861111111110404, -0.1292346314604056468 ) ) ;
#12534 = AXIS2_PLACEMENT_3D ( 'NONE', #10495, #17925, #10612 ) ;
#12535 = CARTESIAN_POINT ( 'NONE',  ( 0.3119999999999999996, 4.859805555707287894, 0.1292346314604056190 ) ) ;
#12536 = ORIENTED_EDGE ( 'NONE', *, *, #4662, .T. ) ;
#12537 = CARTESIAN_POINT ( 'NONE',  ( 0.2530624153226711526, 5.072996518863750026, 0.1824922298374807572 ) ) ;
#12538 = VERTEX_POINT ( 'NONE', #6222 ) ;
#12539 = EDGE_CURVE ( 'NONE', #544, #20226, #13686, .T. ) ;
#12540 = CARTESIAN_POINT ( 'NONE',  ( -0.1899746975659765691, 4.882988235955101786, -0.2474948752168808219 ) ) ;
#12541 = CARTESIAN_POINT ( 'NONE',  ( 0.000000000000000000, 0.3155070326520292845, 0.3296527777777817358 ) ) ;
#12542 = CARTESIAN_POINT ( 'NONE',  ( -0.1167790944451423257, 5.231333333409198261, -0.2819296736111110424 ) ) ;
#12543 = CARTESIAN_POINT ( 'NONE',  ( 5.731347020009612645E-17, 3.953555555555555046, 0.3119999999999999996 ) ) ;
#12544 = EDGE_CURVE ( 'NONE', #7025, #19443, #8710, .T. ) ;
#12545 = CARTESIAN_POINT ( 'NONE',  ( -0.2923287055106771337, 0.3080357141881718275, -0.2123892367102620804 ) ) ;
#12546 = CARTESIAN_POINT ( 'NONE',  ( 0.2819296736111110424, 0.3236111110352444808, 0.1167790944451424923 ) ) ;
#12547 = CARTESIAN_POINT ( 'NONE',  ( -0.1954553509668046640, 0.1954553509668046918, 0.03277777777777921009 ) ) ;
#12548 = CARTESIAN_POINT ( 'NONE',  ( -1.726321361862525858E-17, 5.130638888964754507, -0.2819296736111110979 ) ) ;
#12549 = CARTESIAN_POINT ( 'NONE',  ( 0.3059100320596817579, 4.472671705659782226, 0.06139557928590994029 ) ) ;
#12550 = EDGE_LOOP ( 'NONE', ( #6518, #6785, #4574, #2150 ) ) ;
#12551 = DIRECTION ( 'NONE',  ( -0.000000000000000000, -1.000000000000000000, -0.000000000000000000 ) ) ;
#12552 = CARTESIAN_POINT ( 'NONE',  ( 0.3999999999999999667, 0.1107142857142856956, 0.1299678784931626307 ) ) ;
#12553 = DIRECTION ( 'NONE',  ( 0.000000000000000000, -0.5150380749100555988, -0.8571673007021114454 ) ) ;
#12554 = CARTESIAN_POINT ( 'NONE',  ( 0.1292346314604058410, 4.734805555555555046, 0.3119999999999998885 ) ) ;
#12555 = CARTESIAN_POINT ( 'NONE',  ( 0.1772105346487870270, 5.205904791023236555, 0.2204285013117096848 ) ) ;
#12556 = CC_DESIGN_DATE_AND_TIME_ASSIGNMENT ( #5, #13088, ( #19708 ) ) ;
#12557 = CARTESIAN_POINT ( 'NONE',  ( -0.2819296736111110979, 3.904944444520309865, -0.1167790944451422980 ) ) ;
#12558 = CARTESIAN_POINT ( 'NONE',  ( -0.1993543840281266355, 3.762583333409198705, 0.1993543840281267465 ) ) ;
#12559 = CARTESIAN_POINT ( 'NONE',  ( -0.2206173157302028787, 0.6013888887371559022, 0.2206173157302027954 ) ) ;
#12560 = CARTESIAN_POINT ( 'NONE',  ( -0.009375000000000169656, 0.5358532185916217161, 0.06112444011295373875 ) ) ;
#12561 = ORIENTED_EDGE ( 'NONE', *, *, #22586, .F. ) ;
#12562 = CARTESIAN_POINT ( 'NONE',  ( 0.3119999999999999996, 3.915361111111110848, -0.1292346314604056745 ) ) ;
#12563 = CARTESIAN_POINT ( 'NONE',  ( 0.1993543840281267465, 4.484805555631420582, 0.1993543840281266633 ) ) ;
#12564 = CARTESIAN_POINT ( 'NONE',  ( -0.05415793351760116864, 4.489840156517192149, -0.3074561344383239803 ) ) ;
#12565 = AXIS2_PLACEMENT_3D ( 'NONE', #20097, #13041, #16682 ) ;
#12566 = CALENDAR_DATE ( 2026, 7, 10 ) ;
#12567 = CARTESIAN_POINT ( 'NONE',  ( -0.4593750000000004219, -0.2760455974562901482, 0.06112444011295364160 ) ) ;
#12568 = CARTESIAN_POINT ( 'NONE',  ( -0.1954553509668046640, 0.1954553509668046918, 0.1369444444444467002 ) ) ;
#12569 = CARTESIAN_POINT ( 'NONE',  ( -0.1167790944451423119, 4.078555555631421470, -0.2819296736111110979 ) ) ;
#12570 = DIRECTION ( 'NONE',  ( 1.000000000000000000, 0.000000000000000000, 0.000000000000000000 ) ) ;
#12571 = CARTESIAN_POINT ( 'NONE',  ( 0.4620259694561523744, 0.2880908832651560281, 0.04413116910601654758 ) ) ;
#12572 = CARTESIAN_POINT ( 'NONE',  ( -0.006454613307746792129, -0.5491961284534644383, 0.04193467568257210759 ) ) ;
#12573 = CARTESIAN_POINT ( 'NONE',  ( -6.979263641208234666E-17, 0.06517857133102901435, 0.3799334167787516425 ) ) ;
#12574 = CARTESIAN_POINT ( 'NONE',  ( 0.2819296736111110424, 0.03888888881302225708, -0.1167790944451423119 ) ) ;
#12575 = CARTESIAN_POINT ( 'NONE',  ( 0.4687500000000002776, 0.1743477725058785177, 0.07807923930880629471 ) ) ;
#12576 = CARTESIAN_POINT ( 'NONE',  ( -0.3066867353193226120, 1.999640111863030700, -2.247133083939565790 ) ) ;
#12577 = EDGE_CURVE ( 'NONE', #6211, #23184, #17560, .T. ) ;
#12578 = CARTESIAN_POINT ( 'NONE',  ( -0.007027963641057663469, 0.1556215347031258966, -0.7500000000000003331 ) ) ;
#12579 = CARTESIAN_POINT ( 'NONE',  ( -0.2764156081756484196, 1.692557448933383907E-17, 0.03277777777777921009 ) ) ;
#12580 = CARTESIAN_POINT ( 'NONE',  ( 0.3155070326520292845, -5.795770164686806123E-17, 0.3678472222222261001 ) ) ;
#12581 = ORIENTED_EDGE ( 'NONE', *, *, #1428, .F. ) ;
#12582 = LINE ( 'NONE', #17816, #18454 ) ;
#12583 = CARTESIAN_POINT ( 'NONE',  ( 4.898587196589413075E-17, 3.700000000000000622, 0.4000000000000000222 ) ) ;
#12584 = CARTESIAN_POINT ( 'NONE',  ( -0.3119999999999999996, 0.09791666666666633267, -0.1292346314604056745 ) ) ;
#12585 = CARTESIAN_POINT ( 'NONE',  ( 0.1015005499617950280, 3.738732058664179903, -0.2819296736111110424 ) ) ;
#12586 = CARTESIAN_POINT ( 'NONE',  ( 0.2923287055106771337, 0.09017857133102902267, -0.2123892367102620249 ) ) ;
#12587 = CIRCLE ( 'NONE', #6353, 0.001000000000000037101 ) ;
#12588 = ADVANCED_FACE ( 'NONE', ( #11979 ), #6583, .F. ) ;
#12589 = CARTESIAN_POINT ( 'NONE',  ( 0.2819296736111110424, 4.453555555631421470, -0.1167790944451423396 ) ) ;
#12590 = DIRECTION ( 'NONE',  ( 0.000000000000000000, 5.763336813132313106E-16, 1.000000000000000000 ) ) ;
#12591 = DIRECTION ( 'NONE',  ( -0.5773502691896227335, -0.5773502691896255090, -0.5773502691896290617 ) ) ;
#12592 = B_SPLINE_CURVE_WITH_KNOTS ( 'NONE', 3,
 ( #8729, #14351, #16186, #8981, #23354, #16426, #5191, #23712, #4952, #21424, #3371, #1061, #17891, #18249, #8857, #17767, #21782, #5070, #21541, #12417, #12540, #10695, #14111, #6666, #18131, #6544, #3247, #13994, #1429, #16301, #12661, #19833, #1185, #10823, #10583 ),
 .UNSPECIFIED., .F., .F.,
 ( 4, 2, 2, 2, 2, 2, 2, 2, 1, 2, 2, 1, 1, 2, 2, 2, 2, 2, 4 ),
 ( 0.2101647747907265662, 0.2124489175043063061, 0.2147330602178860459, 0.2170172029314657858, 0.2193013456450455256, 0.2215854883586252655, 0.2238696310722050054, 0.2244406667505999264, 0.2245834256701986775, 0.2246191154000983514, 0.2246280378325732907, 0.2246369602650482022, 0.2246548051299980531, 0.2247261845897974286, 0.2250117024289949308, 0.2255827381073899907, 0.2261537737857850228, 0.2272958451425751147, 0.2284379164993652067 ),
 .UNSPECIFIED. ) ;
#12593 = VERTEX_POINT ( 'NONE', #12336 ) ;
#12594 = CARTESIAN_POINT ( 'NONE',  ( 0.006680993209926284343, 4.376987163322225705, -0.3119999970774108844 ) ) ;
#12595 = CARTESIAN_POINT ( 'NONE',  ( -0.3119999999999999996, 3.720916666818399055, -0.1292346314604056468 ) ) ;
#12596 = CARTESIAN_POINT ( 'NONE',  ( 0.01571168205836896356, 4.210054417711290853, -0.3116595364661075007 ) ) ;
#12597 = LINE ( 'NONE', #2453, #10763 ) ;
#12598 = CARTESIAN_POINT ( 'NONE',  ( -0.2819296736111110979, 4.852861111186976828, 0.000000000000000000 ) ) ;
#12599 = COORDINATED_UNIVERSAL_TIME_OFFSET ( 0, 0, .AHEAD. ) ;
#12600 = ORIENTED_EDGE ( 'NONE', *, *, #4199, .T. ) ;
#12601 = VECTOR ( 'NONE', #12322, 39.37007874015748143 ) ;
#12602 = CARTESIAN_POINT ( 'NONE',  ( -4.760580627680044823E-09, 4.932722222506802368, -0.3119999999999999996 ) ) ;
#12603 = LINE ( 'NONE', #9046, #8108 ) ;
#12604 = EDGE_LOOP ( 'NONE', ( #18466, #23699, #3493, #24069, #12768, #4224, #5997, #22771, #12936, #688 ) ) ;
#12605 = CARTESIAN_POINT ( 'NONE',  ( -0.2819296736111110979, 0.2993055554796889561, -3.452642723725051716E-17 ) ) ;
#12606 = ADVANCED_FACE ( 'NONE', ( #10258 ), #16096, .T. ) ;
#12607 = ADVANCED_FACE ( 'NONE', ( #21575 ), #23510, .T. ) ;
#12608 = VERTEX_POINT ( 'NONE', #976 ) ;
#12609 = CARTESIAN_POINT ( 'NONE',  ( 0.2819296736111110979, 0.1048611110352444808, 0.000000000000000000 ) ) ;
#12610 = CARTESIAN_POINT ( 'NONE',  ( 0.000000000000000000, 0.000000000000000000, 1.326383476483184332 ) ) ;
#12611 = CARTESIAN_POINT ( 'NONE',  ( -0.5116234456863466562, 0.9548081934128056503, 2.549370209580444691 ) ) ;
#12612 = CARTESIAN_POINT ( 'NONE',  ( 0.2472135954999579721, -0.08928571428571427382, -0.3402603233408159622 ) ) ;
#12613 = DIRECTION ( 'NONE',  ( 0.000000000000000000, 0.000000000000000000, -1.000000000000000000 ) ) ;
#12614 = CARTESIAN_POINT ( 'NONE',  ( 0.2998642343065497373, 0.08796414601275419354, 0.4241666666666771834 ) ) ;
#12615 = CARTESIAN_POINT ( 'NONE',  ( -0.2579334647780821554, 3.885737390849240747, -0.1755419818098827023 ) ) ;
#12616 = CARTESIAN_POINT ( 'NONE',  ( -0.5116234456863466562, 0.9548081934128058723, 2.635972749958888528 ) ) ;
#12617 = CARTESIAN_POINT ( 'NONE',  ( -1.726321361862525858E-17, 4.408416666742533074, -0.2819296736111110979 ) ) ;
#12618 = PLANE ( 'NONE',  #10107 ) ;
#12619 = CARTESIAN_POINT ( 'NONE',  ( 0.003701402432584371873, 4.543728254411404599, -0.3119811817425749978 ) ) ;
#12620 = ADVANCED_FACE ( 'NONE', ( #15973 ), #8529, .T. ) ;
#12621 = CARTESIAN_POINT ( 'NONE',  ( -0.1993543840281266910, 5.082027777853643791, -0.1993543840281266910 ) ) ;
#12622 = DIRECTION ( 'NONE',  ( -1.000000000000000000, 0.000000000000000000, 0.000000000000000000 ) ) ;
#12623 = CARTESIAN_POINT ( 'NONE',  ( 0.3119835370037090105, 3.753046293522503074, -0.02992120370447185970 ) ) ;
#12624 = CARTESIAN_POINT ( 'NONE',  ( 0.2468659554013261648, 0.05872605207754656720, 0.1866057693320590238 ) ) ;
#12625 = ORIENTED_EDGE ( 'NONE', *, *, #4146, .T. ) ;
#12626 = CARTESIAN_POINT ( 'NONE',  ( -0.3236067977499789694, 0.2053571426620580398, -0.2351141009169893104 ) ) ;
#12627 = CARTESIAN_POINT ( 'NONE',  ( -0.2206173157302028232, 4.273000000151732536, -0.2206173157302028232 ) ) ;
#12628 = CIRCLE ( 'NONE', #13013, 0.3150000000000000022 ) ;
#12629 = CARTESIAN_POINT ( 'NONE',  ( 0.2819296736111111534, 4.557722222298087544, 0.1167790944451422563 ) ) ;
#12630 = CARTESIAN_POINT ( 'NONE',  ( -0.1167790944451423535, 3.807722222298087988, 0.2819296736111110424 ) ) ;
#12631 = VERTEX_POINT ( 'NONE', #13917 ) ;
#12632 = ORIENTED_EDGE ( 'NONE', *, *, #10547, .F. ) ;
#12633 = VERTEX_POINT ( 'NONE', #17684 ) ;
#12634 = SECURITY_CLASSIFICATION_LEVEL ( 'unclassified' ) ;
#12635 = CARTESIAN_POINT ( 'NONE',  ( 0.2730879860166530726, 3.066692553488282957, 2.936183489075822717 ) ) ;
#12636 = DIRECTION ( 'NONE',  ( -0.000000000000000000, -1.000000000000000000, -0.000000000000000000 ) ) ;
#12637 = ORIENTED_EDGE ( 'NONE', *, *, #8564, .F. ) ;
#12638 = ADVANCED_BREP_SHAPE_REPRESENTATION ( '', ( #1448, #9127 ), #15765 ) ;
#12639 = CARTESIAN_POINT ( 'NONE',  ( -0.3119999999999999996, 0.2611111109593781676, -3.820898013339742174E-17 ) ) ;
#12640 = CARTESIAN_POINT ( 'NONE',  ( 0.3096898932022673079, 0.3624663341596540134, 0.07654795713851909877 ) ) ;
#12641 = CARTESIAN_POINT ( 'NONE',  ( 0.1797085267211815662, 3.721720965436318362, -0.2172307213220433242 ) ) ;
#12642 = CARTESIAN_POINT ( 'NONE',  ( -0.01491610195037358991, 3.710900762300672007, -0.3119999571456253951 ) ) ;
#12643 = VECTOR ( 'NONE', #14432, 39.37007874015748143 ) ;
#12644 = CARTESIAN_POINT ( 'NONE',  ( 0.2233192592356399997, -0.06696428581182808926, -0.3073725909049500049 ) ) ;
#12645 = CARTESIAN_POINT ( 'NONE',  ( 0.09542861826504350775, 0.1770968263373798313, -0.7440186716057061167 ) ) ;
#12646 = ORIENTED_EDGE ( 'NONE', *, *, #4005, .F. ) ;
#12647 = ORIENTED_EDGE ( 'NONE', *, *, #12033, .T. ) ;
#12648 = APPLICATION_CONTEXT ( 'configuration controlled 3d designs of mechanical parts and assemblies' ) ;
#12649 = CARTESIAN_POINT ( 'NONE',  ( 0.1425746527767651484, 5.075825272696307344, 0.2781771577023212649 ) ) ;
#12650 = CARTESIAN_POINT ( 'NONE',  ( 0.2764156081756483641, -0.1144950937579611167, 0.3904166666666709085 ) ) ;
#12651 = EDGE_CURVE ( 'NONE', #7279, #3958, #18688, .T. ) ;
#12652 = CARTESIAN_POINT ( 'NONE',  ( -0.2819296736111110424, 4.134111111186976828, 0.1167790944451424923 ) ) ;
#12653 = CARTESIAN_POINT ( 'NONE',  ( -0.2819296736111110424, 5.023000000075866112, 0.1167790944451424923 ) ) ;
#12654 = CARTESIAN_POINT ( 'NONE',  ( 0.1054825322676819915, -0.2618223909956544082, 0.3934028307984435147 ) ) ;
#12655 = CARTESIAN_POINT ( 'NONE',  ( -0.1099743054185288865, 4.235112341272140313, 0.2928703655857898824 ) ) ;
#12656 = CARTESIAN_POINT ( 'NONE',  ( 5.731347020009612645E-17, 4.009111111111109516, 0.3119999999999999996 ) ) ;
#12657 = CARTESIAN_POINT ( 'NONE',  ( -0.2206173157302028232, 5.050777777929510215, -0.2206173157302028232 ) ) ;
#12658 = CARTESIAN_POINT ( 'NONE',  ( -0.3119999999999999996, 4.158416666666665762, -0.1292346314604056468 ) ) ;
#12659 = ORIENTED_EDGE ( 'NONE', *, *, #20051, .T. ) ;
#12660 = VECTOR ( 'NONE', #14928, 39.37007874015748143 ) ;
#12661 = CARTESIAN_POINT ( 'NONE',  ( -0.05059632256427344654, 4.878606678054476120, -0.3088345630771059946 ) ) ;
#12662 = CARTESIAN_POINT ( 'NONE',  ( -0.2230971623002954152, -0.2230971623002953874, 0.1838194444444472553 ) ) ;
#12663 = CARTESIAN_POINT ( 'NONE',  ( -0.001863919267159286786, 4.559812086079793048, -2.908070964936878333 ) ) ;
#12664 =( GEOMETRIC_REPRESENTATION_CONTEXT ( 3 ) GLOBAL_UNCERTAINTY_ASSIGNED_CONTEXT ( ( #936 ) ) GLOBAL_UNIT_ASSIGNED_CONTEXT ( ( #21959, #7214, #23656 ) ) REPRESENTATION_CONTEXT ( 'NONE', 'WORKASPACE' ) );
#12665 = CARTESIAN_POINT ( 'NONE',  ( 0.4581189881604794678, -0.2644951211353317455, 0.3941886329748525153 ) ) ;
#12666 = PRODUCT_DEFINITION_SHAPE ( 'NONE', 'NONE',  #14477 ) ;
#12667 = CARTESIAN_POINT ( 'NONE',  ( 0.2923287055106771337, 0.3437499999024575814, 0.2123892367102621359 ) ) ;
#12668 = CARTESIAN_POINT ( 'NONE',  ( -0.1167790944451422702, 0.2333333332574666907, -0.2819296736111110979 ) ) ;
#12669 = CARTESIAN_POINT ( 'NONE',  ( 0.1144950937579611444, 0.2764156081756483641, 0.2445833333333364279 ) ) ;
#12670 = ADVANCED_FACE ( 'NONE', ( #6463 ), #1338, .F. ) ;
#12671 = LINE ( 'NONE', #10832, #8184 ) ;
#12672 = DIRECTION ( 'NONE',  ( 0.5773502691896236216, 0.5773502691896299499, -0.5773502691896236216 ) ) ;
#12673 = AXIS2_PLACEMENT_3D ( 'NONE', #18856, #4089, #11782 ) ;
#12674 = ORIENTED_EDGE ( 'NONE', *, *, #20163, .F. ) ;
#12675 = EDGE_CURVE ( 'NONE', #9702, #2053, #13836, .T. ) ;
#12676 = CARTESIAN_POINT ( 'NONE',  ( 0.7919466436700954848, 2.665000000000000036, -2.986000000000000210 ) ) ;
#12677 = CARTESIAN_POINT ( 'NONE',  ( -0.005017074662756174433, 4.599534034751092015, -0.3119621811286065194 ) ) ;
#12678 = CARTESIAN_POINT ( 'NONE',  ( 0.06049446539525574207, 4.875506709053786913, -0.3065030800618469553 ) ) ;
#12679 = CARTESIAN_POINT ( 'NONE',  ( 8.375559671162349491E-15, 3.988277777929486678, -0.3119999999999999996 ) ) ;
#12680 = CARTESIAN_POINT ( 'NONE',  ( 0.3124999999999999445, 0.1294417382415923023, 0.3140277777777812362 ) ) ;
#12681 = CARTESIAN_POINT ( 'NONE',  ( -0.3119999999999998885, 4.776472222222222008, 0.1292346314604058410 ) ) ;
#12682 = CARTESIAN_POINT ( 'NONE',  ( -0.1993543840281266910, 4.012583333409198261, -0.1993543840281266910 ) ) ;
#12683 = CARTESIAN_POINT ( 'NONE',  ( 0.2819296736111110424, 3.842444444520310309, -0.1167790944451423396 ) ) ;
#12684 = CARTESIAN_POINT ( 'NONE',  ( 0.2935269953798502751, 4.032991781582652813, -0.1057786308535565989 ) ) ;
#12685 = CARTESIAN_POINT ( 'NONE',  ( 1.457716030923678074, 2.291712385858714729, -2.174029041877829194 ) ) ;
#12686 = SECURITY_CLASSIFICATION ( '', '', #8643 ) ;
#12687 = ORIENTED_EDGE ( 'NONE', *, *, #20031, .F. ) ;
#12688 = CARTESIAN_POINT ( 'NONE',  ( 0.006674681701965033860, -0.5374122480878900099, 0.05975678175779891577 ) ) ;
#12689 = CARTESIAN_POINT ( 'NONE',  ( -0.2819296736111110979, 4.519527777853643791, 0.000000000000000000 ) ) ;
#12690 = CARTESIAN_POINT ( 'NONE',  ( 0.2206173157302027954, 3.807722222222221564, -0.2206173157302028232 ) ) ;
#12691 = AXIS2_PLACEMENT_3D ( 'NONE', #21905, #10702, #1434 ) ;
#12692 = CARTESIAN_POINT ( 'NONE',  ( -0.4687500000000003886, -0.2598076211353319009, 0.06112444011295369711 ) ) ;
#12693 = CARTESIAN_POINT ( 'NONE',  ( 0.2764156081756483641, -0.1144950937579611167, 0.3348611111111149952 ) ) ;
#12694 = CARTESIAN_POINT ( 'NONE',  ( -0.1167790944451423119, 3.800777777853643347, -0.2819296736111110979 ) ) ;
#12695 = DIRECTION ( 'NONE',  ( -1.000000000000000000, 0.000000000000000000, 0.000000000000000000 ) ) ;
#12696 = CARTESIAN_POINT ( 'NONE',  ( 0.07873564497862947653, 5.159726166786684054, -0.2898521741972847621 ) ) ;
#12697 = PRODUCT_RELATED_PRODUCT_CATEGORY ( 'detail', '', ( #23325 ) ) ;
#12698 = DIRECTION ( 'NONE',  ( 0.000000000000000000, 0.000000000000000000, -1.000000000000000000 ) ) ;
#12699 = B_SPLINE_CURVE_WITH_KNOTS ( 'NONE', 3,
 ( #2024, #7628, #5796, #20677, #3969, #11417, #2146, #17015, #19916, #1852, #23672, #16384, #16736, #7349, #8811, #23913, #12859, #20033, #20155, #16502, #1737, #12615, #21860, #16620, #7466, #7234, #5029, #22098, #1621, #20396, #12979, #14553, #20277, #9055, #3687, #14434, #9296, #12496, #11134, #18441, #10651, #24040, #3563, #3322, #18324, #16260 ),
 .UNSPECIFIED., .F., .F.,
 ( 4, 2, 2, 2, 2, 2, 2, 2, 2, 2, 2, 1, 1, 2, 2, 1, 1, 1, 1, 2, 2, 2, 2, 2, 2, 4 ),
 ( 0.8613901642458987595, 0.8629494678102641592, 0.8645087713746295588, 0.8660680749389949584, 0.8676273785033603581, 0.8691866820677257577, 0.8707459856320911573, 0.8723052891964565569, 0.8738645927608219566, 0.8769831998895527558, 0.8801018070182835551, 0.8804916329093749328, 0.8806865458549205661, 0.8807109099731137425, 0.8807139554878878895, 0.8807170010026620366, 0.8807230920322103307, 0.8807352740913069189, 0.8807840023276931607, 0.8808814588004657553, 0.8816611105826461792, 0.8824407623648266030, 0.8832204141470070269, 0.8840000659291875618, 0.8847797177113679856, 0.8863390212757288333 ),
 .UNSPECIFIED. ) ;
#12700 = APPROVAL_PERSON_ORGANIZATION ( #911, #1200, #4803 ) ;
#12701 = CARTESIAN_POINT ( 'NONE',  ( 0.3613381517857143232, 0.08303571418817186356, 0.000000000000000000 ) ) ;
#12702 = CARTESIAN_POINT ( 'NONE',  ( -0.1993543840281266633, 0.2229166665908000333, -0.1993543840281266910 ) ) ;
#12703 = CARTESIAN_POINT ( 'NONE',  ( 2.034975993999860866E-05, 3.877166120065549837, -0.3120000000214913638 ) ) ;
#12704 = CARTESIAN_POINT ( 'NONE',  ( 0.3806690758928571450, 0.4111607142369430590, 0.000000000000000000 ) ) ;
#12705 = CARTESIAN_POINT ( 'NONE',  ( -0.1394808293864866489, 0.5344994213878939693, -0.7369348578741334865 ) ) ;
#12706 = CARTESIAN_POINT ( 'NONE',  ( 0.1954553509668047195, 0.1954553509668046085, 0.06750000000000172529 ) ) ;
#12707 = CARTESIAN_POINT ( 'NONE',  ( 0.2764156081756484196, -5.077672346800151106E-17, 0.06750000000000168365 ) ) ;
#12708 = ORIENTED_EDGE ( 'NONE', *, *, #19200, .F. ) ;
#12709 = ORIENTED_EDGE ( 'NONE', *, *, #3707, .F. ) ;
#12710 = CARTESIAN_POINT ( 'NONE',  ( 0.01848103877824584448, 0.5441716683897389606, 0.04413116910601658227 ) ) ;
#12711 = CARTESIAN_POINT ( 'NONE',  ( 0.4584464601845412712, -0.2220115010439547287, 0.4062888617107747180 ) ) ;
#12712 = CARTESIAN_POINT ( 'NONE',  ( 0.1993543840281266910, 0.5979166665908001166, -0.1993543840281266910 ) ) ;
#12713 = CARTESIAN_POINT ( 'NONE',  ( 0.1167790944451422702, 3.793833333409199149, -0.2819296736111110424 ) ) ;
#12714 = CARTESIAN_POINT ( 'NONE',  ( -0.3613381517857144343, 0.1937499999024576147, 0.1174058825155740171 ) ) ;
#12715 = CIRCLE ( 'NONE', #19298, 0.2499999999999999722 ) ;
#12716 = CARTESIAN_POINT ( 'NONE',  ( -0.1993543840281266910, 4.359805555631421470, -0.1993543840281266910 ) ) ;
#12717 = CARTESIAN_POINT ( 'NONE',  ( 0.1292346314604039537, 4.957027777777777366, 0.3120000000000016649 ) ) ;
#12718 = CARTESIAN_POINT ( 'NONE',  ( -0.3119999999999999996, 4.606333333333332725, 0.000000000000000000 ) ) ;
#12719 = ORIENTED_EDGE ( 'NONE', *, *, #18544, .T. ) ;
#12720 = CARTESIAN_POINT ( 'NONE',  ( 0.2246729631343395983, 4.370108299028268917, -0.2176007414103741100 ) ) ;
#12721 = CARTESIAN_POINT ( 'NONE',  ( -1.726321361862525858E-17, 5.227861111186975940, -0.2819296736111110979 ) ) ;
#12722 = SECURITY_CLASSIFICATION ( '', '', #17592 ) ;
#12723 = CARTESIAN_POINT ( 'NONE',  ( 0.0009908759922620817475, 4.210471905009121052, -0.3119986526024096096 ) ) ;
#12724 = CARTESIAN_POINT ( 'NONE',  ( -0.2206173157302028232, 4.988277777777777366, -0.2206173157302028232 ) ) ;
#12725 = VECTOR ( 'NONE', #23547, 39.37007874015748143 ) ;
#12726 = CARTESIAN_POINT ( 'NONE',  ( 0.1167790944451424506, 4.814666666742533074, 0.2819296736111110424 ) ) ;
#12727 = CONTEXT_DEPENDENT_SHAPE_REPRESENTATION ( #3903, #23933 ) ;
#12728 = EDGE_CURVE ( 'NONE', #16124, #3616, #19589, .T. ) ;
#12729 = CARTESIAN_POINT ( 'NONE',  ( -0.1794086211558035826, 4.066157371076530858, 0.2554475641543275666 ) ) ;
#12730 = CARTESIAN_POINT ( 'NONE',  ( 0.2977072594216367274, -5.468793635004571549E-17, -0.08687392608830331320 ) ) ;
#12731 = VERTEX_POINT ( 'NONE', #19392 ) ;
#12732 = CARTESIAN_POINT ( 'NONE',  ( -0.2819296736111110979, 0.3027777777019111660, 0.1167790944451422425 ) ) ;
#12733 = CARTESIAN_POINT ( 'NONE',  ( 1.726321361862525858E-17, 0.3409722221463556413, -0.2819296736111110979 ) ) ;
#12734 = CARTESIAN_POINT ( 'NONE',  ( -0.09855069764300931900, 4.713304858131104780, -0.2968621023885956167 ) ) ;
#12735 = CARTESIAN_POINT ( 'NONE',  ( -0.1985766828738846912, 5.195784807567790153, -0.2074211384348365605 ) ) ;
#12736 = CARTESIAN_POINT ( 'NONE',  ( 0.2233192592356399164, 0.4116071427596004750, 0.3073725909049500604 ) ) ;
#12737 = CARTESIAN_POINT ( 'NONE',  ( 0.1306872919485614071, -0.3155070326520293955, -0.03145833333333261650 ) ) ;
#12738 =( BOUNDED_CURVE ( )  B_SPLINE_CURVE ( 2, ( #22202, #3429, #14785, #7099, #18547, #14537, #1837, #16722, #21960, #2, #5013, #12479, #19898 ),
 .UNSPECIFIED., .F., .T. ) 
 B_SPLINE_CURVE_WITH_KNOTS ( ( 3, 2, 2, 2, 2, 2, 3 ),
 ( 0.5357142857142856984, 0.5428571428571428159, 0.5571428571428571619, 0.5714285714285713969, 0.5857142857142857428, 0.5999999999999999778, 0.6071428571428572063 ),
 .UNSPECIFIED. ) 
 CURVE ( )  GEOMETRIC_REPRESENTATION_ITEM ( )  RATIONAL_B_SPLINE_CURVE ( ( 0.9755282581475768211, 0.9755282581475768211, 1.000000000000000000, 0.9510565162951535312, 1.000000000000000000, 0.9510565162951535312, 1.000000000000000000, 0.9510565162951535312, 1.000000000000000000, 0.9510565162951535312, 1.000000000000000000, 0.9755282581475765991, 0.9755282581475768211 ) ) 
 REPRESENTATION_ITEM ( '' )  );
#12739 = DIRECTION ( 'NONE',  ( 0.8660254037844524744, 0.000000000000000000, -0.4999999999999761857 ) ) ;
#12740 = FACE_OUTER_BOUND ( 'NONE', #14931, .T. ) ;
#12741 = ORGANIZATION ( 'NAUO-ORG8', 'UNSPECIFIED', 'UNSPECIFIED' ) ;
#12742 = CARTESIAN_POINT ( 'NONE',  ( 0.1993543840281266355, 0.08402777770191115214, 0.1993543840281267465 ) ) ;
#12743 = CARTESIAN_POINT ( 'NONE',  ( -0.1167790944451423535, 4.599388888964754507, 0.2819296736111110424 ) ) ;
#12744 = FACE_OUTER_BOUND ( 'NONE', #19330, .T. ) ;
#12745 = CARTESIAN_POINT ( 'NONE',  ( 0.3128595373675272517, 4.529777549056624331, 0.005372927980562640198 ) ) ;
#12746 = CARTESIAN_POINT ( 'NONE',  ( 0.1167790944451422702, 5.016055555631420582, -0.2819296736111110424 ) ) ;
#12747 = CARTESIAN_POINT ( 'NONE',  ( 0.4687500000000003886, -0.08745052389986661401, 0.08858773447093017117 ) ) ;
#12748 = CARTESIAN_POINT ( 'NONE',  ( 0.2497132334490027028, 4.924618274614680047, -0.1914511699637774511 ) ) ;
#12749 = CARTESIAN_POINT ( 'NONE',  ( 0.02752505417202956439, 0.04140457188012223316, 0.2899247665489211312 ) ) ;
#12750 = AXIS2_PLACEMENT_3D ( 'NONE', #19874, #8411, #23044 ) ;
#12751 = CARTESIAN_POINT ( 'NONE',  ( -0.1965595339002992048, 0.4277821775562039019, 0.07944544255962410206 ) ) ;
#12752 = CARTESIAN_POINT ( 'NONE',  ( -0.3119999999999998885, 4.394527777929509327, 0.1292346314604058410 ) ) ;
#12753 = CARTESIAN_POINT ( 'NONE',  ( 0.1167790944451424506, 4.550777777853644679, 0.2819296736111110424 ) ) ;
#12754 = CARTESIAN_POINT ( 'NONE',  ( -0.1167790944451423535, 3.918833333409198705, 0.2819296736111110424 ) ) ;
#12755 = ORIENTED_EDGE ( 'NONE', *, *, #23237, .F. ) ;
#12756 = ORIENTED_EDGE ( 'NONE', *, *, #24094, .F. ) ;
#12757 = CALENDAR_DATE ( 2026, 7, 10 ) ;
#12758 = EDGE_CURVE ( 'NONE', #21481, #13713, #19627, .T. ) ;
#12759 = CARTESIAN_POINT ( 'NONE',  ( -0.1919110571530789344, 4.938596203506701698, -0.2493703182469045598 ) ) ;
#12760 = CARTESIAN_POINT ( 'NONE',  ( 3.025220084236446727, 2.291712385858714729, -2.986000000000001098 ) ) ;
#12761 = ORIENTED_EDGE ( 'NONE', *, *, #11886, .F. ) ;
#12762 = CARTESIAN_POINT ( 'NONE',  ( 0.2206173157302027676, 0.2819444442927114824, 0.2206173157302028787 ) ) ;
#12763 = VECTOR ( 'NONE', #13690, 39.37007874015748854 ) ;
#12764 = CARTESIAN_POINT ( 'NONE',  ( 0.4872114317030045716, 0.000000000000000000, -1.140285115251740145 ) ) ;
#12765 = CARTESIAN_POINT ( 'NONE',  ( -0.2041014093529595619, 5.123076492009982275, 0.2308277784739024285 ) ) ;
#12766 = CARTESIAN_POINT ( 'NONE',  ( 2.986000000000000210, 0.05000000000000028727, -2.541000000000000369 ) ) ;
#12767 = CARTESIAN_POINT ( 'NONE',  ( 0.03519696264514372147, 0.1583449576561939409, -0.7492059971800684171 ) ) ;
#12768 = ORIENTED_EDGE ( 'NONE', *, *, #6236, .F. ) ;
#12769 = ORIENTED_EDGE ( 'NONE', *, *, #16756, .F. ) ;
#12770 = CARTESIAN_POINT ( 'NONE',  ( 0.08891876399603607095, 5.074138123154654068, 0.2996821340870129413 ) ) ;
#12771 = CARTESIAN_POINT ( 'NONE',  ( 0.1144950937579611444, 0.2764156081756483641, 0.2931944444444479769 ) ) ;
#12772 = CARTESIAN_POINT ( 'NONE',  ( 0.2819296736111110979, 4.321611111186976828, 0.1167790944451422425 ) ) ;
#12773 = CARTESIAN_POINT ( 'NONE',  ( -0.1167790944451423119, 5.064666666742532186, -0.2819296736111110979 ) ) ;
#12774 = EDGE_CURVE ( 'NONE', #18008, #22560, #10143, .T. ) ;
#12775 = CARTESIAN_POINT ( 'NONE',  ( 0.05416907386903872107, -0.2729753724328379261, 0.3894056226408110222 ) ) ;
#12776 = CARTESIAN_POINT ( 'NONE',  ( 0.1292346314604056190, 3.977861111111111292, -0.3119999999999999996 ) ) ;
#12777 = CARTESIAN_POINT ( 'NONE',  ( -0.3119999999999999996, 4.998694444596177178, -0.1292346314604056468 ) ) ;
#12778 = CARTESIAN_POINT ( 'NONE',  ( 0.1167790944451422702, 5.071611111186976828, -0.2819296736111110979 ) ) ;
#12779 = EDGE_CURVE ( 'NONE', #7806, #17266, #21802, .T. ) ;
#12780 = AXIS2_PLACEMENT_3D ( 'NONE', #7531, #17038, #9365 ) ;
#12781 = CARTESIAN_POINT ( 'NONE',  ( 0.01874999999999976685, 0.5520911949125799634, 0.06112444011295372487 ) ) ;
#12782 = CARTESIAN_POINT ( 'NONE',  ( 0.1419551320365925184, -0.2751926619865908696, 0.4208614314731936590 ) ) ;
#12783 =( BOUNDED_SURFACE ( )  B_SPLINE_SURFACE ( 1, 2, ( 
 ( #6660, #19583, #21660, #2532, #4822, #2876, #10099, #21302, #13755, #4595, #13990, #11805, #6302, #2650, #4708, #6539, #13873, #9978, #19226, #17405, #23471, #19466, #21180, #17762, #12176, #10335, #19352, #1056, #8484, #8616, #698, #11934, #15926, #19706, #3008, #10459, #17885, #16056, #15575, #22999, #17521, #816, #15696, #3126, #21897, #10579, #9091, #5187, #5314, #14842, #12657, #23831, #23960, #5064, #8852, #16178, #12901, #18125, #7389, #16298, #20075, #1424, #16659, #3601, #18244, #12777, #16423, #19954, #23591, #7032, #21778, #12413, #14474, #23710, #3364, #10817, #7153, #14594, #10691, #22016, #18363, #1542, #20197, #10935, #7273, #3484, #20317, #14721, #18007, #1656, #4948, #8974, #1775, #19831, #16541, #11053, #18482, #9221, #24082, #22136, #5436, #1300, #8724, #6907, #14346, #12535, #3243, #22497, #16776, #2387, #9340, #2265, #5676, #14955, #9700, #542, #17011, #22258, #15188, #9578, #20909, #13257, #16891, #5911, #18844, #13495, #7507, #19080, #5554, #4203, #11536, #3730, #1898, #304, #3966, #20789, #7745, #11657, #4080, #17258, #9824, #15075, #2021, #7624, #11177, #18605, #17139, #7978, #11410, #63, #11294, #22625, #13368, #9459, #18968, #184, #13019, #2141, #20673, #5793, #426, #20434, #22375, #13141, #20554, #22738, #7860, #15309, #18723, #6026, #3850, #21027, #23082, #19437, #15785, #4681, #4796, #19677, #13727, #19324, #12151, #2622, #21149, #6391, #10188, #13962, #10065, #8456, #17490, #19557, #21392, #23321, #2848, #15429, #4319, #10434, #15899, #22856, #23203, #10307, #15546, #784, #17731, #1025, #8214, #21272, #6629, #2737, #4437, #13843, #14077, #21506, #12262, #2980, #15663, #9944, #17858, #4564, #12023, #22968, #902, #6514, #1150, #6145, #17374, #17612, #8334, #13612, #11774, #19194, #2504, #664, #8093, #6269, #11904, #14446, #6752, #1393, #14197, #12752, #8824, #8947, #18453, #16270, #3333, #3455, #8697, #12506, #19803, #16512, #21753, #11027, #19927, #23682, #5039, #20289, #7246, #21870, #16395, #20044, #23564, #3100, #10660, #1271, #16025, #18092, #3214, #7003, #5161, #10790, #18217, #14320, #1512, #21989, #12627, #23803, #14564, #10907, #20168, #16149, #7124, #5284, #18336, #1631, #9065, #3574, #6878, #8588, #23926, #14692, #22110, #23441, #5405, #10546, #12872, #21631, #4923, #12387, #17980, #9550, #16749, #16868, #13229, #22596, #5769, #5880, #20642, #13340, #155, #24051, #18693, #11629, #11146, #15281, #7597, #16633, #9430, #31, #20526, #7478, #12992, #20762, #16985, #1748, #7361, #4053, #277, #14926, #11266, #3699, #1993, #3941, #4175, #20406, #22345, #11383, #22472, #3823, #14812, #20881, #9190, #2240, #7716, #15163, #11507, #17109, #18943, #22228, #9672, #5528, #13112, #22709, #18576, #15049, #399, #7835, #5999, #1867, #18812, #2109, #5647, #9307, #13465, #8069, #19292, #15521, #2597, #13589, #23292, #6121, #23177, #2480, #11751, #6487, #21483, #13815, #19056, #12000, #6367, #17705, #10043, #13706, #2711, #15642, #10283, #4295, #15875, #2360, #999, #8310, #514, #22831, #21249, #757, #17587, #4538, #8429, #879, #14053, #6605, #11877, #22943, #4415, #7948, #15402, #13938, #4768, #8188, #21001, #6243, #19412, #10164, #21124, #15761, #17466, #9800, #23059, #21368, #4654, #12125, #17232, #19174, #9915, #17346, #19532, #2826, #640, #8668, #10757, #21727, #17832, #19894, #16242, #12595, #1483, #1605, #16484, #10517, #16119 ),
 ( #8920, #12239, #1121, #7211, #12721, #19651, #20015, #16362, #12357, #5011, #18187, #23773, #12474, #18061, #7096, #23654, #17950, #3185, #21840, #3302, #9039, #14657, #14169, #1361, #5128, #14534, #10634, #20137, #21956, #23893, #8790, #5250, #21600, #6972, #10407, #14414, #8555, #3427, #10877, #18306, #22078, #2949, #15998, #23416, #19776, #23532, #6727, #4894, #1243, #3072, #6849, #14290, #1833, #17074, #4027, #18662, #13199, #16840, #20376, #24021, #7449, #22198, #12840, #14896, #16719, #3790, #11236, #125, #15018, #11114, #7568, #18782, #22316, #20613, #11355, #250, #16952, #5498, #1957, #20495, #22440, #5740, #3910, #366, #12962, #7808, #20730, #22562, #9401, #20259, #2210, #7332, #4125, #15249, #7685, #9156, #2079, #9518, #3666, #15136, #5853, #13314, #11475, #18908, #9641, #5374, #3546, #10997, #5614, #18425, #14783, #1718, #16601, #18543, #13078, #9278, #17316, #13560, #9764, #10132, #6332, #8393, #13432, #17556, #13787, #20971, #8041, #486, #15490, #730, #963, #17201, #4268, #8158, #19260, #609, #20853, #17676, #5969, #10248, #9888, #7919, #4505, #13678, #22919, #6091, #850, #19499, #6213, #21214, #15371, #4384, #4145, #21092, #11599, #2682, #11842, #23031, #22679, #2564, #17435, #8278, #22798, #2447, #11717, #6454, #19141, #19031, #10012, #15611, #11970, #2327, #21335, #19384, #15729, #23143, #13907, #4624, #12089, #2794, #23263, #1211, #3039, #14258, #21692, #10604, #1330, #21566, #3154, #5095, #17917, #23624, #21807, #10724, #3271, #8520, #12443, #6815, #18033, #16211, #8756, #10847, #15960, #18277, #7064, #8886, #4974, #6573, #12689, #10370, #10486, #3397, #18156, #19618, #6938, #14377, #6691, #19858, #12563, #19983, #1452, #16329, #23739, #14502, #21924, #14023, #8641, #1572, #1088, #5215, #20107, #21454, #23500, #14136, #16088, #4859, #2913, #15844, #4737, #12209, #17795, #23383, #12325, #19740, #18847, #10970, #2145, #11540, #11777, #3519, #186, #18971, #5914, #3968, #23863, #4323, #16451, #21030, #20676, #18394, #15313, #308, #11415, #16894, #2268, #9703, #22859, #19198, #1690, #15191, #17142, #11660, #7748, #9827, #22629, #9582, #430, #13373, #545, #9124, #6149, #9008, #7980, #22742, #14627, #12810, #20794, #4083, #7863, #6031, #15433, #13498, #7185, #13615, #17014, #13260, #20913, #22050, #5346, #4206, #20230, #19083, #7627, #22498, #2391, #17262, #15078, #5795, #13846, #4926, #6517, #17615, #21276, #4800, #16029, #21634, #22971, #17861, #2983, #907, #6633, #23086, #1029, #12027, #8096, #10192, #13965, #2852, #15902, #23445, #6756, #788, #6394, #23324, #4567, #8217, #8336, #21396, #8459, #19440, #19680, #2740, #14081, #21509, #10437, #12265, #2507, #15550, #12389, #1153, #9947, #10312, #8591, #2625, #15788, #14202, #17377, #23205, #4684, #669, #12154, #15667, #19561, #6273, #13730, #21153, #17734, #4440, #11907, #19327, #10069, #17493, #7005, #16635, #10550, #8949, #18456, #1751, #3576, #14814, #20046, #12754, #1395, #17983, #14448, #8826, #3336, #16272, #10792, #14322, #24053, #6882, #23932, #3217, #12508, #7248, #22233, #14568, #19806, #20170, #7126, #9193, #5286, #22112, #18220, #20291, #14694, #7363, #5164, #18338, #5041, #1516, #1274, #12630, #8702, #5407, #16397, #3458, #5530, #23805, #21991, #12874, #19931, #23684, #21755, #11029, #21872, #3103, #10909, #1633, #9067, #16152, #23567, #16515, #10663, #18096, #3825, #7481, #15050 ) ),
 .UNSPECIFIED., .F., .F., .T. ) 
 B_SPLINE_SURFACE_WITH_KNOTS ( ( 2, 2 ),
 ( 3, 2, 2, 2, 2, 2, 2, 2, 2, 2, 2, 2, 2, 2, 2, 2, 2, 2, 2, 2, 2, 2, 2, 2, 2, 2, 2, 2, 2, 2, 2, 2, 2, 2, 2, 2, 2, 2, 2, 2, 2, 2, 2, 2, 2, 2, 2, 2, 2, 2, 2, 2, 2, 2, 2, 2, 2, 2, 2, 2, 2, 2, 2, 2, 2, 2, 2, 2, 2, 2, 2, 2, 2, 2, 2, 2, 2, 2, 2, 2, 2, 2, 2, 2, 2, 2, 2, 2, 2, 2, 2, 2, 2, 2, 2, 2, 2, 2, 2, 2, 2, 2, 2, 2, 2, 2, 2, 2, 2, 2, 2, 2, 2, 2, 2, 2, 2, 2, 2, 2, 2, 2, 2, 2, 2, 2, 2, 2, 2, 2, 2, 2, 2, 2, 2, 2, 2, 2, 2, 2, 2, 2, 2, 2, 2, 2, 2, 2, 2, 2, 2, 2, 2, 2, 2, 2, 2, 2, 2, 2, 2, 2, 2, 2, 2, 2, 2, 2, 2, 2, 2, 2, 2, 2, 2, 2, 2, 2, 2, 2, 2, 2, 2, 2, 2, 2, 2, 2, 2, 2, 2, 2, 2, 2, 2, 2, 2, 2, 2, 2, 2, 2, 2, 2, 2, 2, 2, 2, 2, 2, 2, 2, 2, 2, 2, 2, 2, 2, 2, 3 ),
 ( 0.000000000000000000, 1.000000000000000000 ),
 ( 0.000000000000000000, 0.004464285714285714038, 0.008928571428571428076, 0.01339285714285714211, 0.01785714285714285615, 0.02232142857142857192, 0.02678571428571428423, 0.03125000000000000000, 0.03571428571428571230, 0.04017857142857143155, 0.04464285714285714385, 0.04910714285714285615, 0.05357142857142856845, 0.05803571428571428770, 0.06250000000000000000, 0.06696428571428571230, 0.07142857142857142461, 0.07589285714285713691, 0.08035714285714286309, 0.08482142857142857539, 0.08928571428571428770, 0.09375000000000000000, 0.09821428571428571230, 0.1026785714285714246, 0.1071428571428571369, 0.1116071428571428631, 0.1160714285714285754, 0.1205357142857142877, 0.1250000000000000000, 0.1294642857142857262, 0.1339285714285714246, 0.1383928571428571508, 0.1428571428571428492, 0.1473214285714285754, 0.1517857142857142738, 0.1562500000000000000, 0.1607142857142857262, 0.1651785714285714246, 0.1696428571428571508, 0.1741071428571428492, 0.1785714285714285754, 0.1830357142857142738, 0.1875000000000000000, 0.1919642857142857262, 0.1964285714285714246, 0.2008928571428571508, 0.2053571428571428492, 0.2098214285714285754, 0.2142857142857142738, 0.2187500000000000000, 0.2232142857142857262, 0.2276785714285714246, 0.2321428571428571508, 0.2366071428571428492, 0.2410714285714285754, 0.2455357142857142738, 0.2500000000000000000, 0.2544642857142856984, 0.2589285714285714524, 0.2633928571428571508, 0.2678571428571428492, 0.2723214285714285476, 0.2767857142857143016, 0.2812500000000000000, 0.2857142857142856984, 0.2901785714285714524, 0.2946428571428571508, 0.2991071428571428492, 0.3035714285714285476, 0.3080357142857143016, 0.3125000000000000000, 0.3169642857142856984, 0.3214285714285714524, 0.3258928571428571508, 0.3303571428571428492, 0.3348214285714285476, 0.3392857142857143016, 0.3437500000000000000, 0.3482142857142856984, 0.3526785714285714524, 0.3571428571428571508, 0.3616071428571428492, 0.3660714285714285476, 0.3705357142857143016, 0.3750000000000000000, 0.3794642857142856984, 0.3839285714285714524, 0.3883928571428571508, 0.3928571428571428492, 0.3973214285714285476, 0.4017857142857143016, 0.4062500000000000000, 0.4107142857142856984, 0.4151785714285714524, 0.4196428571428571508, 0.4241071428571428492, 0.4285714285714285476, 0.4330357142857143016, 0.4375000000000000000, 0.4419642857142856984, 0.4464285714285714524, 0.4508928571428571508, 0.4553571428571428492, 0.4598214285714285476, 0.4642857142857143016, 0.4687500000000000000, 0.4732142857142856984, 0.4776785714285714524, 0.4821428571428571508, 0.4866071428571428492, 0.4910714285714285476, 0.4955357142857143016, 0.5000000000000000000, 0.5044642857142856984, 0.5089285714285713969, 0.5133928571428570953, 0.5178571428571429047, 0.5223214285714286031, 0.5267857142857143016, 0.5312500000000000000, 0.5357142857142856984, 0.5401785714285713969, 0.5446428571428570953, 0.5491071428571429047, 0.5535714285714286031, 0.5580357142857143016, 0.5625000000000000000, 0.5669642857142856984, 0.5714285714285713969, 0.5758928571428570953, 0.5803571428571429047, 0.5848214285714286031, 0.5892857142857143016, 0.5937500000000000000, 0.5982142857142856984, 0.6026785714285713969, 0.6071428571428570953, 0.6116071428571429047, 0.6160714285714286031, 0.6205357142857143016, 0.6250000000000000000, 0.6294642857142856984, 0.6339285714285713969, 0.6383928571428570953, 0.6428571428571429047, 0.6473214285714286031, 0.6517857142857143016, 0.6562500000000000000, 0.6607142857142856984, 0.6651785714285713969, 0.6696428571428570953, 0.6741071428571429047, 0.6785714285714286031, 0.6830357142857143016, 0.6875000000000000000, 0.6919642857142856984, 0.6964285714285713969, 0.7008928571428570953, 0.7053571428571429047, 0.7098214285714286031, 0.7142857142857143016, 0.7187500000000000000, 0.7232142857142856984, 0.7276785714285713969, 0.7321428571428570953, 0.7366071428571429047, 0.7410714285714286031, 0.7455357142857143016, 0.7500000000000000000, 0.7544642857142856984, 0.7589285714285713969, 0.7633928571428570953, 0.7678571428571429047, 0.7723214285714286031, 0.7767857142857143016, 0.7812500000000000000, 0.7857142857142856984, 0.7901785714285713969, 0.7946428571428570953, 0.7991071428571429047, 0.8035714285714286031, 0.8080357142857143016, 0.8125000000000000000, 0.8169642857142856984, 0.8214285714285713969, 0.8258928571428570953, 0.8303571428571429047, 0.8348214285714286031, 0.8392857142857143016, 0.8437500000000000000, 0.8482142857142856984, 0.8526785714285713969, 0.8571428571428570953, 0.8616071428571429047, 0.8660714285714286031, 0.8705357142857143016, 0.8750000000000000000, 0.8794642857142856984, 0.8839285714285713969, 0.8883928571428570953, 0.8928571428571429047, 0.8973214285714286031, 0.9017857142857143016, 0.9062500000000000000, 0.9107142857142856984, 0.9151785714285713969, 0.9196428571428570953, 0.9241071428571429047, 0.9285714285714286031, 0.9330357142857143016, 0.9375000000000000000, 0.9419642857142856984, 0.9464285714285713969, 0.9508928571428570953, 0.9553571428571429047, 0.9598214285714286031, 0.9642857142857143016, 0.9687500000000000000, 0.9732142857142856984, 0.9771335305660339143 ),
 .UNSPECIFIED. ) 
 GEOMETRIC_REPRESENTATION_ITEM ( )  RATIONAL_B_SPLINE_SURFACE ( (
 ( 1.000000000000000000, 0.9238795325112867385, 1.000000000000000000, 0.9238795325112867385, 1.000000000000000000, 0.9238795325112867385, 1.000000000000000000, 0.9238795325112867385, 1.000000000000000000, 0.9238795325112867385, 1.000000000000000000, 0.9238795325112867385, 1.000000000000000000, 0.9238795325112867385, 1.000000000000000000, 0.9238795325112867385, 1.000000000000000000, 0.9238795325112867385, 1.000000000000000000, 0.9238795325112867385, 1.000000000000000000, 0.9238795325112867385, 1.000000000000000000, 0.9238795325112867385, 1.000000000000000000, 0.9238795325112867385, 1.000000000000000000, 0.9238795325112867385, 1.000000000000000000, 0.9238795325112867385, 1.000000000000000000, 0.9238795325112867385, 1.000000000000000000, 0.9238795325112867385, 1.000000000000000000, 0.9238795325112867385, 1.000000000000000000, 0.9238795325112867385, 1.000000000000000000, 0.9238795325112867385, 1.000000000000000000, 0.9238795325112867385, 1.000000000000000000, 0.9238795325112867385, 1.000000000000000000, 0.9238795325112867385, 1.000000000000000000, 0.9238795325112867385, 1.000000000000000000, 0.9238795325112867385, 1.000000000000000000, 0.9238795325112867385, 1.000000000000000000, 0.9238795325112867385, 1.000000000000000000, 0.9238795325112867385, 1.000000000000000000, 0.9238795325112867385, 1.000000000000000000, 0.9238795325112867385, 1.000000000000000000, 0.9238795325112867385, 1.000000000000000000, 0.9238795325112867385, 1.000000000000000000, 0.9238795325112867385, 1.000000000000000000, 0.9238795325112867385, 1.000000000000000000, 0.9238795325112867385, 1.000000000000000000, 0.9238795325112867385, 1.000000000000000000, 0.9238795325112867385, 1.000000000000000000, 0.9238795325112867385, 1.000000000000000000, 0.9238795325112867385, 1.000000000000000000, 0.9238795325112867385, 1.000000000000000000, 0.9238795325112867385, 1.000000000000000000, 0.9238795325112867385, 1.000000000000000000, 0.9238795325112867385, 1.000000000000000000, 0.9238795325112867385, 1.000000000000000000, 0.9238795325112867385, 1.000000000000000000, 0.9238795325112867385, 1.000000000000000000, 0.9238795325112867385, 1.000000000000000000, 0.9238795325112867385, 1.000000000000000000, 0.9238795325112867385, 1.000000000000000000, 0.9238795325112867385, 1.000000000000000000, 0.9238795325112867385, 1.000000000000000000, 0.9238795325112867385, 1.000000000000000000, 0.9238795325112867385, 1.000000000000000000, 0.9238795325112867385, 1.000000000000000000, 0.9238795325112867385, 1.000000000000000000, 0.9238795325112867385, 1.000000000000000000, 0.9238795325112867385, 1.000000000000000000, 0.9238795325112867385, 1.000000000000000000, 0.9238795325112867385, 1.000000000000000000, 0.9238795325112867385, 1.000000000000000000, 0.9238795325112867385, 1.000000000000000000, 0.9238795325112867385, 1.000000000000000000, 0.9238795325112867385, 1.000000000000000000, 0.9238795325112867385, 1.000000000000000000, 0.9238795325112867385, 1.000000000000000000, 0.9238795325112867385, 1.000000000000000000, 0.9238795325112867385, 1.000000000000000000, 0.9238795325112867385, 1.000000000000000000, 0.9238795325112867385, 1.000000000000000000, 0.9238795325112867385, 1.000000000000000000, 0.9238795325112867385, 1.000000000000000000, 0.9238795325112867385, 1.000000000000000000, 0.9238795325112867385, 1.000000000000000000, 0.9238795325112867385, 1.000000000000000000, 0.9238795325112867385, 1.000000000000000000, 0.9238795325112867385, 1.000000000000000000, 0.9238795325112867385, 1.000000000000000000, 0.9238795325112867385, 1.000000000000000000, 0.9238795325112867385, 1.000000000000000000, 0.9238795325112867385, 1.000000000000000000, 0.9238795325112867385, 1.000000000000000000, 0.9238795325112867385, 1.000000000000000000, 0.9238795325112867385, 1.000000000000000000, 0.9238795325112867385, 1.000000000000000000, 0.9238795325112867385, 1.000000000000000000, 0.9238795325112867385, 1.000000000000000000, 0.9238795325112867385, 1.000000000000000000, 0.9238795325112867385, 1.000000000000000000, 0.9238795325112867385, 1.000000000000000000, 0.9238795325112867385, 1.000000000000000000, 0.9238795325112867385, 1.000000000000000000, 0.9238795325112867385, 1.000000000000000000, 0.9238795325112867385, 1.000000000000000000, 0.9238795325112867385, 1.000000000000000000, 0.9238795325112867385, 1.000000000000000000, 0.9238795325112867385, 1.000000000000000000, 0.9238795325112867385, 1.000000000000000000, 0.9238795325112867385, 1.000000000000000000, 0.9238795325112867385, 1.000000000000000000, 0.9238795325112867385, 1.000000000000000000, 0.9238795325112867385, 1.000000000000000000, 0.9238795325112867385, 1.000000000000000000, 0.9238795325112867385, 1.000000000000000000, 0.9238795325112867385, 1.000000000000000000, 0.9238795325112867385, 1.000000000000000000, 0.9238795325112867385, 1.000000000000000000, 0.9238795325112867385, 1.000000000000000000, 0.9238795325112867385, 1.000000000000000000, 0.9238795325112867385, 1.000000000000000000, 0.9238795325112867385, 1.000000000000000000, 0.9238795325112867385, 1.000000000000000000, 0.9238795325112867385, 1.000000000000000000, 0.9238795325112867385, 1.000000000000000000, 0.9238795325112867385, 1.000000000000000000, 0.9238795325112867385, 1.000000000000000000, 0.9238795325112867385, 1.000000000000000000, 0.9238795325112867385, 1.000000000000000000, 0.9238795325112867385, 1.000000000000000000, 0.9238795325112867385, 1.000000000000000000, 0.9238795325112867385, 1.000000000000000000, 0.9238795325112867385, 1.000000000000000000, 0.9238795325112867385, 1.000000000000000000, 0.9238795325112867385, 1.000000000000000000, 0.9238795325112867385, 1.000000000000000000, 0.9238795325112867385, 1.000000000000000000, 0.9238795325112867385, 1.000000000000000000, 0.9238795325112867385, 1.000000000000000000, 0.9238795325112867385, 1.000000000000000000, 0.9238795325112867385, 1.000000000000000000, 0.9238795325112867385, 1.000000000000000000, 0.9238795325112867385, 1.000000000000000000, 0.9238795325112867385, 1.000000000000000000, 0.9238795325112867385, 1.000000000000000000, 0.9238795325112867385, 1.000000000000000000, 0.9238795325112867385, 1.000000000000000000, 0.9238795325112867385, 1.000000000000000000, 0.9238795325112867385, 1.000000000000000000, 0.9238795325112867385, 1.000000000000000000, 0.9238795325112867385, 1.000000000000000000, 0.9238795325112867385, 1.000000000000000000, 0.9238795325112867385, 1.000000000000000000, 0.9238795325112867385, 1.000000000000000000, 0.9238795325112867385, 1.000000000000000000, 0.9238795325112867385, 1.000000000000000000, 0.9238795325112867385, 1.000000000000000000, 0.9238795325112867385, 1.000000000000000000, 0.9238795325112867385, 1.000000000000000000, 0.9238795325112867385, 1.000000000000000000, 0.9238795325112867385, 1.000000000000000000, 0.9238795325112867385, 1.000000000000000000, 0.9238795325112867385, 1.000000000000000000, 0.9238795325112867385, 1.000000000000000000, 0.9238795325112867385, 1.000000000000000000, 0.9238795325112867385, 1.000000000000000000, 0.9238795325112867385, 1.000000000000000000, 0.9238795325112867385, 1.000000000000000000, 0.9238795325112867385, 1.000000000000000000, 0.9238795325112867385, 1.000000000000000000, 0.9238795325112867385, 1.000000000000000000, 0.9238795325112867385, 1.000000000000000000, 0.9238795325112867385, 1.000000000000000000, 0.9238795325112867385, 1.000000000000000000, 0.9238795325112867385, 1.000000000000000000, 0.9238795325112867385, 1.000000000000000000, 0.9238795325112867385, 1.000000000000000000, 0.9238795325112867385, 1.000000000000000000, 0.9238795325112867385, 1.000000000000000000, 0.9238795325112867385, 1.000000000000000000, 0.9238795325112867385, 1.000000000000000000, 0.9238795325112867385, 1.000000000000000000, 0.9238795325112867385, 1.000000000000000000, 0.9238795325112867385, 1.000000000000000000, 0.9238795325112867385, 1.000000000000000000, 0.9238795325112867385, 1.000000000000000000, 0.9238795325112867385, 1.000000000000000000, 0.9238795325112867385, 1.000000000000000000, 0.9238795325112867385, 1.000000000000000000, 0.9238795325112867385, 1.000000000000000000, 0.9238795325112867385, 1.000000000000000000, 0.9238795325112867385, 1.000000000000000000, 0.9238795325112867385, 1.000000000000000000, 0.9238795325112867385, 1.000000000000000000, 0.9238795325112867385, 1.000000000000000000, 0.9238795325112867385, 1.000000000000000000, 0.9238795325112867385, 1.000000000000000000, 0.9238795325112867385, 1.000000000000000000, 0.9238795325112867385, 1.000000000000000000, 0.9238795325112867385, 1.000000000000000000, 0.9238795325112867385, 1.000000000000000000, 0.9238795325112867385, 1.000000000000000000, 0.9238795325112867385, 1.000000000000000000, 0.9238795325112867385, 1.000000000000000000, 0.9238795325112867385, 1.000000000000000000, 0.9238795325112867385, 1.000000000000000000, 0.9238795325112867385, 1.000000000000000000, 0.9238795325112867385, 1.000000000000000000, 0.9238795325112867385, 1.000000000000000000, 0.9238795325112867385, 1.000000000000000000, 0.9238795325112867385, 1.000000000000000000, 0.9238795325112867385, 1.000000000000000000, 0.9238795325112867385, 1.000000000000000000, 0.9238795325112867385, 1.000000000000000000, 0.9238795325112867385, 1.000000000000000000, 0.9238795325112867385, 1.000000000000000000, 0.9238795325112867385, 1.000000000000000000, 0.9238795325112867385, 1.000000000000000000, 0.9238795325112867385, 1.000000000000000000, 0.9238795325112867385, 1.000000000000000000, 0.9238795325112867385, 1.000000000000000000, 0.9238795325112867385, 1.000000000000000000, 0.9238795325112867385, 1.000000000000000000, 0.9238795325112867385, 1.000000000000000000, 0.9238795325112867385, 1.000000000000000000, 0.9238795325112867385, 1.000000000000000000, 0.9238795325112867385, 1.000000000000000000, 0.9238795325112867385, 1.000000000000000000, 0.9238795325112867385, 1.000000000000000000, 0.9238795325112867385, 1.000000000000000000, 0.9331730159288109672, 0.9836823002065551158),
 ( 1.000000000000000000, 0.9238795325112867385, 1.000000000000000000, 0.9238795325112867385, 1.000000000000000000, 0.9238795325112867385, 1.000000000000000000, 0.9238795325112867385, 1.000000000000000000, 0.9238795325112867385, 1.000000000000000000, 0.9238795325112867385, 1.000000000000000000, 0.9238795325112867385, 1.000000000000000000, 0.9238795325112867385, 1.000000000000000000, 0.9238795325112867385, 1.000000000000000000, 0.9238795325112867385, 1.000000000000000000, 0.9238795325112867385, 1.000000000000000000, 0.9238795325112867385, 1.000000000000000000, 0.9238795325112867385, 1.000000000000000000, 0.9238795325112867385, 1.000000000000000000, 0.9238795325112867385, 1.000000000000000000, 0.9238795325112867385, 1.000000000000000000, 0.9238795325112867385, 1.000000000000000000, 0.9238795325112867385, 1.000000000000000000, 0.9238795325112867385, 1.000000000000000000, 0.9238795325112867385, 1.000000000000000000, 0.9238795325112867385, 1.000000000000000000, 0.9238795325112867385, 1.000000000000000000, 0.9238795325112867385, 1.000000000000000000, 0.9238795325112867385, 1.000000000000000000, 0.9238795325112867385, 1.000000000000000000, 0.9238795325112867385, 1.000000000000000000, 0.9238795325112867385, 1.000000000000000000, 0.9238795325112867385, 1.000000000000000000, 0.9238795325112867385, 1.000000000000000000, 0.9238795325112867385, 1.000000000000000000, 0.9238795325112867385, 1.000000000000000000, 0.9238795325112867385, 1.000000000000000000, 0.9238795325112867385, 1.000000000000000000, 0.9238795325112867385, 1.000000000000000000, 0.9238795325112867385, 1.000000000000000000, 0.9238795325112867385, 1.000000000000000000, 0.9238795325112867385, 1.000000000000000000, 0.9238795325112867385, 1.000000000000000000, 0.9238795325112867385, 1.000000000000000000, 0.9238795325112867385, 1.000000000000000000, 0.9238795325112867385, 1.000000000000000000, 0.9238795325112867385, 1.000000000000000000, 0.9238795325112867385, 1.000000000000000000, 0.9238795325112867385, 1.000000000000000000, 0.9238795325112867385, 1.000000000000000000, 0.9238795325112867385, 1.000000000000000000, 0.9238795325112867385, 1.000000000000000000, 0.9238795325112867385, 1.000000000000000000, 0.9238795325112867385, 1.000000000000000000, 0.9238795325112867385, 1.000000000000000000, 0.9238795325112867385, 1.000000000000000000, 0.9238795325112867385, 1.000000000000000000, 0.9238795325112867385, 1.000000000000000000, 0.9238795325112867385, 1.000000000000000000, 0.9238795325112867385, 1.000000000000000000, 0.9238795325112867385, 1.000000000000000000, 0.9238795325112867385, 1.000000000000000000, 0.9238795325112867385, 1.000000000000000000, 0.9238795325112867385, 1.000000000000000000, 0.9238795325112867385, 1.000000000000000000, 0.9238795325112867385, 1.000000000000000000, 0.9238795325112867385, 1.000000000000000000, 0.9238795325112867385, 1.000000000000000000, 0.9238795325112867385, 1.000000000000000000, 0.9238795325112867385, 1.000000000000000000, 0.9238795325112867385, 1.000000000000000000, 0.9238795325112867385, 1.000000000000000000, 0.9238795325112867385, 1.000000000000000000, 0.9238795325112867385, 1.000000000000000000, 0.9238795325112867385, 1.000000000000000000, 0.9238795325112867385, 1.000000000000000000, 0.9238795325112867385, 1.000000000000000000, 0.9238795325112867385, 1.000000000000000000, 0.9238795325112867385, 1.000000000000000000, 0.9238795325112867385, 1.000000000000000000, 0.9238795325112867385, 1.000000000000000000, 0.9238795325112867385, 1.000000000000000000, 0.9238795325112867385, 1.000000000000000000, 0.9238795325112867385, 1.000000000000000000, 0.9238795325112867385, 1.000000000000000000, 0.9238795325112867385, 1.000000000000000000, 0.9238795325112867385, 1.000000000000000000, 0.9238795325112867385, 1.000000000000000000, 0.9238795325112867385, 1.000000000000000000, 0.9238795325112867385, 1.000000000000000000, 0.9238795325112867385, 1.000000000000000000, 0.9238795325112867385, 1.000000000000000000, 0.9238795325112867385, 1.000000000000000000, 0.9238795325112867385, 1.000000000000000000, 0.9238795325112867385, 1.000000000000000000, 0.9238795325112867385, 1.000000000000000000, 0.9238795325112867385, 1.000000000000000000, 0.9238795325112867385, 1.000000000000000000, 0.9238795325112867385, 1.000000000000000000, 0.9238795325112867385, 1.000000000000000000, 0.9238795325112867385, 1.000000000000000000, 0.9238795325112867385, 1.000000000000000000, 0.9238795325112867385, 1.000000000000000000, 0.9238795325112867385, 1.000000000000000000, 0.9238795325112867385, 1.000000000000000000, 0.9238795325112867385, 1.000000000000000000, 0.9238795325112867385, 1.000000000000000000, 0.9238795325112867385, 1.000000000000000000, 0.9238795325112867385, 1.000000000000000000, 0.9238795325112867385, 1.000000000000000000, 0.9238795325112867385, 1.000000000000000000, 0.9238795325112867385, 1.000000000000000000, 0.9238795325112867385, 1.000000000000000000, 0.9238795325112867385, 1.000000000000000000, 0.9238795325112867385, 1.000000000000000000, 0.9238795325112867385, 1.000000000000000000, 0.9238795325112867385, 1.000000000000000000, 0.9238795325112867385, 1.000000000000000000, 0.9238795325112867385, 1.000000000000000000, 0.9238795325112867385, 1.000000000000000000, 0.9238795325112867385, 1.000000000000000000, 0.9238795325112867385, 1.000000000000000000, 0.9238795325112867385, 1.000000000000000000, 0.9238795325112867385, 1.000000000000000000, 0.9238795325112867385, 1.000000000000000000, 0.9238795325112867385, 1.000000000000000000, 0.9238795325112867385, 1.000000000000000000, 0.9238795325112867385, 1.000000000000000000, 0.9238795325112867385, 1.000000000000000000, 0.9238795325112867385, 1.000000000000000000, 0.9238795325112867385, 1.000000000000000000, 0.9238795325112867385, 1.000000000000000000, 0.9238795325112867385, 1.000000000000000000, 0.9238795325112867385, 1.000000000000000000, 0.9238795325112867385, 1.000000000000000000, 0.9238795325112867385, 1.000000000000000000, 0.9238795325112867385, 1.000000000000000000, 0.9238795325112867385, 1.000000000000000000, 0.9238795325112867385, 1.000000000000000000, 0.9238795325112867385, 1.000000000000000000, 0.9238795325112867385, 1.000000000000000000, 0.9238795325112867385, 1.000000000000000000, 0.9238795325112867385, 1.000000000000000000, 0.9238795325112867385, 1.000000000000000000, 0.9238795325112867385, 1.000000000000000000, 0.9238795325112867385, 1.000000000000000000, 0.9238795325112867385, 1.000000000000000000, 0.9238795325112867385, 1.000000000000000000, 0.9238795325112867385, 1.000000000000000000, 0.9238795325112867385, 1.000000000000000000, 0.9238795325112867385, 1.000000000000000000, 0.9238795325112867385, 1.000000000000000000, 0.9238795325112867385, 1.000000000000000000, 0.9238795325112867385, 1.000000000000000000, 0.9238795325112867385, 1.000000000000000000, 0.9238795325112867385, 1.000000000000000000, 0.9238795325112867385, 1.000000000000000000, 0.9238795325112867385, 1.000000000000000000, 0.9238795325112867385, 1.000000000000000000, 0.9238795325112867385, 1.000000000000000000, 0.9238795325112867385, 1.000000000000000000, 0.9238795325112867385, 1.000000000000000000, 0.9238795325112867385, 1.000000000000000000, 0.9238795325112867385, 1.000000000000000000, 0.9238795325112867385, 1.000000000000000000, 0.9238795325112867385, 1.000000000000000000, 0.9238795325112867385, 1.000000000000000000, 0.9238795325112867385, 1.000000000000000000, 0.9238795325112867385, 1.000000000000000000, 0.9238795325112867385, 1.000000000000000000, 0.9238795325112867385, 1.000000000000000000, 0.9238795325112867385, 1.000000000000000000, 0.9238795325112867385, 1.000000000000000000, 0.9238795325112867385, 1.000000000000000000, 0.9238795325112867385, 1.000000000000000000, 0.9238795325112867385, 1.000000000000000000, 0.9238795325112867385, 1.000000000000000000, 0.9238795325112867385, 1.000000000000000000, 0.9238795325112867385, 1.000000000000000000, 0.9238795325112867385, 1.000000000000000000, 0.9238795325112867385, 1.000000000000000000, 0.9238795325112867385, 1.000000000000000000, 0.9238795325112867385, 1.000000000000000000, 0.9238795325112867385, 1.000000000000000000, 0.9238795325112867385, 1.000000000000000000, 0.9238795325112867385, 1.000000000000000000, 0.9238795325112867385, 1.000000000000000000, 0.9238795325112867385, 1.000000000000000000, 0.9238795325112867385, 1.000000000000000000, 0.9238795325112867385, 1.000000000000000000, 0.9238795325112867385, 1.000000000000000000, 0.9238795325112867385, 1.000000000000000000, 0.9238795325112867385, 1.000000000000000000, 0.9238795325112867385, 1.000000000000000000, 0.9238795325112867385, 1.000000000000000000, 0.9238795325112867385, 1.000000000000000000, 0.9238795325112867385, 1.000000000000000000, 0.9238795325112867385, 1.000000000000000000, 0.9238795325112867385, 1.000000000000000000, 0.9238795325112867385, 1.000000000000000000, 0.9238795325112867385, 1.000000000000000000, 0.9238795325112867385, 1.000000000000000000, 0.9238795325112867385, 1.000000000000000000, 0.9238795325112867385, 1.000000000000000000, 0.9238795325112867385, 1.000000000000000000, 0.9238795325112867385, 1.000000000000000000, 0.9238795325112867385, 1.000000000000000000, 0.9238795325112867385, 1.000000000000000000, 0.9238795325112867385, 1.000000000000000000, 0.9238795325112867385, 1.000000000000000000, 0.9238795325112867385, 1.000000000000000000, 0.9238795325112867385, 1.000000000000000000, 0.9238795325112867385, 1.000000000000000000, 0.9238795325112867385, 1.000000000000000000, 0.9238795325112867385, 1.000000000000000000, 0.9238795325112867385, 1.000000000000000000, 0.9238795325112867385, 1.000000000000000000, 0.9238795325112867385, 1.000000000000000000, 0.9238795325112867385, 1.000000000000000000, 0.9238795325112867385, 1.000000000000000000, 0.9238795325112867385, 1.000000000000000000, 0.9238795325112867385, 1.000000000000000000, 0.9238795325112867385, 1.000000000000000000, 0.9331730159288109672, 0.9836823002065551158) ) ) 
 REPRESENTATION_ITEM ( '' )  SURFACE ( )  );
#12784 = CARTESIAN_POINT ( 'NONE',  ( -0.1983289933404564775, 0.05677534557590641767, 0.2335968120589810293 ) ) ;
#12785 = ORIENTED_EDGE ( 'NONE', *, *, #6361, .T. ) ;
#12786 = EDGE_CURVE ( 'NONE', #15581, #8592, #16281, .T. ) ;
#12787 = CARTESIAN_POINT ( 'NONE',  ( 0.000000000000000000, 0.3155070326520292845, 0.1629861111111137739 ) ) ;
#12788 = CARTESIAN_POINT ( 'NONE',  ( -0.1993543840281266355, 5.026472222298088433, 0.1993543840281267465 ) ) ;
#12789 = CARTESIAN_POINT ( 'NONE',  ( 1.750236327630675537E-16, 0.02499999999999997710, 0.3999999999999999667 ) ) ;
#12790 = CARTESIAN_POINT ( 'NONE',  ( -0.2923287055106771337, 0.3794642856167432798, -0.2123892367102620804 ) ) ;
#12791 = VECTOR ( 'NONE', #19378, 39.37007874015748143 ) ;
#12792 = CARTESIAN_POINT ( 'NONE',  ( 0.1993543840281266355, 0.2090277777019111383, 0.1993543840281267465 ) ) ;
#12793 = CARTESIAN_POINT ( 'NONE',  ( -0.2764156081756484196, 1.692557448933383907E-17, 0.2063888888888917028 ) ) ;
#12794 = CARTESIAN_POINT ( 'NONE',  ( -0.2819296736111110424, 5.203555555631421470, 0.1167790944451424923 ) ) ;
#12795 = CARTESIAN_POINT ( 'NONE',  ( 0.05068837741648516554, 5.073009555618063438, 0.3078549794868774558 ) ) ;
#12796 = VERTEX_POINT ( 'NONE', #14760 ) ;
#12797 = CARTESIAN_POINT ( 'NONE',  ( 0.2819296736111110424, 4.995222222298087544, -0.1167790944451423396 ) ) ;
#12798 = CARTESIAN_POINT ( 'NONE',  ( -0.2495230188188473364, 4.174703235102065868, 0.1917148675851489681 ) ) ;
#12799 = CARTESIAN_POINT ( 'NONE',  ( 0.07748689081482018626, 4.875025410756610889, -0.3027932829829018124 ) ) ;
#12800 = CARTESIAN_POINT ( 'NONE',  ( 0.1292346314604033708, 4.568138888888888971, 0.3120000000000023865 ) ) ;
#12801 = CARTESIAN_POINT ( 'NONE',  ( -0.02441201398334205686, 3.066692553488282957, 3.451468604327566858 ) ) ;
#12802 = CARTESIAN_POINT ( 'NONE',  ( -0.2206173157302028232, 4.654944444444443441, -0.2206173157302028232 ) ) ;
#12803 = CARTESIAN_POINT ( 'NONE',  ( 0.2819296736111110979, 4.106333333409199149, -0.1167790944451423396 ) ) ;
#12804 = CARTESIAN_POINT ( 'NONE',  ( -0.2819296736111110979, 3.755638888964754951, 0.000000000000000000 ) ) ;
#12805 = CARTESIAN_POINT ( 'NONE',  ( 0.2961762452215840891, 4.032756265542360552, -0.09810037269422101913 ) ) ;
#12806 = CARTESIAN_POINT ( 'NONE',  ( -5.731347020009612645E-17, 0.2749999998482670627, 0.3119999999999999996 ) ) ;
#12807 = VERTEX_POINT ( 'NONE', #9017 ) ;
#12808 = CARTESIAN_POINT ( 'NONE',  ( 5.731347020009612645E-17, 3.897999999999999243, 0.3119999999999999996 ) ) ;
#12809 = ORIENTED_EDGE ( 'NONE', *, *, #11214, .T. ) ;
#12810 = CARTESIAN_POINT ( 'NONE',  ( -0.1167790944451423535, 4.252166666742533074, 0.2819296736111110424 ) ) ;
#12811 = CARTESIAN_POINT ( 'NONE',  ( -0.3096714640854181244, 4.501118225121650163, -0.03805883575092474519 ) ) ;
#12812 = CONICAL_SURFACE ( 'NONE', #8483, 0.3119999999999999996, 0.7853981633974450594 ) ;
#12813 = ADVANCED_FACE ( 'NONE', ( #22056 ), #22177, .F. ) ;
#12814 = EDGE_CURVE ( 'NONE', #13967, #8952, #19470, .T. ) ;
#12815 = DIRECTION ( 'NONE',  ( -0.8651979924482607887, 0.04370253788966922681, 0.4995222938423283243 ) ) ;
#12816 = CARTESIAN_POINT ( 'NONE',  ( -0.1144950937579609779, 0.2764156081756484196, 0.2445833333333364834 ) ) ;
#12817 = CARTESIAN_POINT ( 'NONE',  ( -0.2494960936497209736, 3.952398630088741260, 0.1917385281361134730 ) ) ;
#12818 = CARTESIAN_POINT ( 'NONE',  ( -0.04084137789490534937, 4.433892237992067997, -0.3099887041510316910 ) ) ;
#12819 = CARTESIAN_POINT ( 'NONE',  ( -0.01848103877824600061, -0.5441716683897390716, 0.04413116910601655452 ) ) ;
#12820 = CARTESIAN_POINT ( 'NONE',  ( 0.2923287055106771337, 0.2330357141881718441, -0.2123892367102620249 ) ) ;
#12821 = CARTESIAN_POINT ( 'NONE',  ( -0.1993543840281267465, 0.1812499999241333759, 0.1993543840281266633 ) ) ;
#12822 = CARTESIAN_POINT ( 'NONE',  ( 0.1917423854131830863, 3.871439620893523337, -0.2494933204621729017 ) ) ;
#12823 = DIRECTION ( 'NONE',  ( -0.000000000000000000, -1.000000000000000000, -0.000000000000000000 ) ) ;
#12824 = CARTESIAN_POINT ( 'NONE',  ( -1.910449006669871087E-17, 4.036888888888888083, -0.3119999999999999996 ) ) ;
#12825 = CARTESIAN_POINT ( 'NONE',  ( 0.000000000000000000, 0.2764156081756484196, -0.1408333333333332826 ) ) ;
#12826 = ORIENTED_EDGE ( 'NONE', *, *, #1131, .T. ) ;
#12827 = VERTEX_POINT ( 'NONE', #12942 ) ;
#12828 = CARTESIAN_POINT ( 'NONE',  ( -0.1807484698107602594, 5.097407819853565059, -0.2533385039640153047 ) ) ;
#12829 = CARTESIAN_POINT ( 'NONE',  ( 0.4687500000000195954, 0.08968933634053308235, 0.4243607940295692216 ) ) ;
#12830 = CARTESIAN_POINT ( 'NONE',  ( -5.178964085587577574E-17, 0.5770833332574667462, 0.2819296736111110979 ) ) ;
#12831 = CARTESIAN_POINT ( 'NONE',  ( 0.1993543840281266633, 3.901472222298087988, -0.1993543840281266910 ) ) ;
#12832 = VECTOR ( 'NONE', #5422, 39.37007874015748854 ) ;
#12833 = CARTESIAN_POINT ( 'NONE',  ( -0.1116596296178199582, 0.3187499999024575592, -0.3436530038418508792 ) ) ;
#12834 = ORIENTED_EDGE ( 'NONE', *, *, #7686, .F. ) ;
#12835 = CARTESIAN_POINT ( 'NONE',  ( 0.1993543840281267465, 4.498694444520309865, 0.1993543840281266633 ) ) ;
#12836 = DIRECTION ( 'NONE',  ( 0.000000000000000000, 0.000000000000000000, 1.000000000000000000 ) ) ;
#12837 = CARTESIAN_POINT ( 'NONE',  ( -1.910449006669871087E-17, 4.592444444444443441, -0.3119999999999999996 ) ) ;
#12838 = EDGE_LOOP ( 'NONE', ( #24088, #5055, #2506, #3621 ) ) ;
#12839 = CARTESIAN_POINT ( 'NONE',  ( 0.2778757787820582137, 4.359068954902455495, 0.1421744276038705013 ) ) ;
#12840 = CARTESIAN_POINT ( 'NONE',  ( -0.1993543840281266355, 5.026472222298088433, 0.1993543840281267465 ) ) ;
#12841 = CARTESIAN_POINT ( 'NONE',  ( 0.3068634962433764435, 4.194799344920210338, 0.06402122387849780438 ) ) ;
#12842 =( CONVERSION_BASED_UNIT ( 'INCH', #5376 ) LENGTH_UNIT ( ) NAMED_UNIT ( #19748 ) );
#12843 = CARTESIAN_POINT ( 'NONE',  ( -0.3119999999999999996, 4.995222222222221120, 0.000000000000000000 ) ) ;
#12844 = VECTOR ( 'NONE', #13287, 39.37007874015748143 ) ;
#12845 = CARTESIAN_POINT ( 'NONE',  ( 0.2819296736111110979, 4.713972222298087544, -3.452642723725051716E-17 ) ) ;
#12846 = DATE_AND_TIME ( #7219, #17764 ) ;
#12847 = CARTESIAN_POINT ( 'NONE',  ( -1.910449006669871087E-17, 4.759111111111110404, -0.3119999999999999996 ) ) ;
#12848 = CARTESIAN_POINT ( 'NONE',  ( -2.750539236387841874E-07, 4.266055563097283176, -0.3119999999998787632 ) ) ;
#12849 = EDGE_CURVE ( 'NONE', #6190, #9761, #8955, .T. ) ;
#12850 = CARTESIAN_POINT ( 'NONE',  ( -0.2819296736111110979, 0.4694444443685776847, 0.1167790944451422425 ) ) ;
#12851 = ORIENTED_EDGE ( 'NONE', *, *, #14495, .T. ) ;
#12852 = ORIENTED_EDGE ( 'NONE', *, *, #23208, .F. ) ;
#12853 = CARTESIAN_POINT ( 'NONE',  ( -0.2819296736111110979, 0.1361111110352444808, 0.1167790944451422425 ) ) ;
#12854 = CARTESIAN_POINT ( 'NONE',  ( -0.3119999999999999996, 4.328555555555554157, 0.000000000000000000 ) ) ;
#12855 = CARTESIAN_POINT ( 'NONE',  ( -0.5116234456863466562, 2.661589509557314326, 2.549370209580444691 ) ) ;
#12856 = CARTESIAN_POINT ( 'NONE',  ( 0.3999999999999999667, 0.04642857142857139546, -0.1299678784931625475 ) ) ;
#12857 = CARTESIAN_POINT ( 'NONE',  ( 0.000000000000000000, 5.954200000000001936, 0.000000000000000000 ) ) ;
#12858 = CARTESIAN_POINT ( 'NONE',  ( 0.1292346314604080892, 4.200083333333331836, -0.3119999999999975016 ) ) ;
#12859 = CARTESIAN_POINT ( 'NONE',  ( -0.3042511176241679549, 3.889013863588333564, -0.07042807391908939563 ) ) ;
#12860 = CARTESIAN_POINT ( 'NONE',  ( 5.731347020009612645E-17, 4.009111111111109516, 0.3119999999999999996 ) ) ;
#12861 = CARTESIAN_POINT ( 'NONE',  ( 0.2819296736111110424, 4.564666666742532186, -0.1167790944451423396 ) ) ;
#12862 = CARTESIAN_POINT ( 'NONE',  ( 0.3999999999999999667, 0.1017857140906294894, 0.1299678784931626307 ) ) ;
#12863 = CARTESIAN_POINT ( 'NONE',  ( 0.1292346314604043700, 4.755638888888888083, -0.3120000000000012763 ) ) ;
#12864 = EDGE_CURVE ( 'NONE', #19381, #644, #7073, .T. ) ;
#12865 = CARTESIAN_POINT ( 'NONE',  ( -1.726321361862525858E-17, 5.186194444520309865, -0.2819296736111110979 ) ) ;
#12866 = CARTESIAN_POINT ( 'NONE',  ( 0.1167790944451422702, 4.557722222298087544, -0.2819296736111110979 ) ) ;
#12867 = CARTESIAN_POINT ( 'NONE',  ( 0.2494037671505511811, 4.913117397265690300, 0.1918541382674933959 ) ) ;
#12868 = CARTESIAN_POINT ( 'NONE',  ( -0.4581189881604794678, 0.2644951211353315235, 0.3941886329748525153 ) ) ;
#12869 = CIRCLE ( 'NONE', #13624, 0.03000000000000002318 ) ;
#12870 = CYLINDRICAL_SURFACE ( 'NONE', #11688, 0.2500000000000000000 ) ;
#12871 = APPROVAL ( #18313, 'UNKNOWN' ) ;
#12872 = CARTESIAN_POINT ( 'NONE',  ( 0.2206173157302027954, 4.203555555707287894, -0.2206173157302028232 ) ) ;
#12873 = CARTESIAN_POINT ( 'NONE',  ( -0.2819296736111110424, 4.592444444520309865, 0.1167790944451424923 ) ) ;
#12874 = CARTESIAN_POINT ( 'NONE',  ( 0.1167790944451422702, 3.779944444520310309, -0.2819296736111110424 ) ) ;
#12875 = ORIENTED_EDGE ( 'NONE', *, *, #6401, .T. ) ;
#12876 = PRODUCT_DEFINITION_SHAPE ( 'NONE', 'NONE',  #24134 ) ;
#12877 = EDGE_LOOP ( 'NONE', ( #20024, #11448, #14065, #3027 ) ) ;
#12878 = ORIENTED_EDGE ( 'NONE', *, *, #5216, .F. ) ;
#12879 = APPLICATION_PROTOCOL_DEFINITION ( 'international standard', 'config_control_design', 1994, #2977 ) ;
#12880 = CARTESIAN_POINT ( 'NONE',  ( 0.4620259694561340003, -0.2880908832651663531, 0.04413116910602139092 ) ) ;
#12881 = AXIS2_PLACEMENT_3D ( 'NONE', #16805, #8998, #5334 ) ;
#12882 = CARTESIAN_POINT ( 'NONE',  ( 0.2206173157302027954, 4.252166666666665762, -0.2206173157302028232 ) ) ;
#12883 = DIRECTION ( 'NONE',  ( 0.000000000000000000, 0.000000000000000000, -1.000000000000000000 ) ) ;
#12884 = ORIENTED_EDGE ( 'NONE', *, *, #22259, .T. ) ;
#12885 = CARTESIAN_POINT ( 'NONE',  ( 0.2206173157302028232, 0.1847222220704893003, -0.2206173157302028232 ) ) ;
#12886 = AXIS2_PLACEMENT_3D ( 'NONE', #10103, #13992, #17526 ) ;
#12887 = CARTESIAN_POINT ( 'NONE',  ( -0.2209708691207961373, -0.2209708691207961095, 0.1855555555555583880 ) ) ;
#12888 = CARTESIAN_POINT ( 'NONE',  ( -0.1224332991792908831, 3.734713384307907447, 0.2872374373138953940 ) ) ;
#12889 = DIRECTION ( 'NONE',  ( 0.5773502691896322814, -0.5773502691896258421, -0.5773502691896191807 ) ) ;
#12890 = CARTESIAN_POINT ( 'NONE',  ( 0.009632836665255781541, 5.167574349600237760, 0.2973209551366967074 ) ) ;
#12891 = ORIENTED_EDGE ( 'NONE', *, *, #19918, .F. ) ;
#12892 = CARTESIAN_POINT ( 'NONE',  ( -0.3613381517857143788, 0.1223214284738861485, 0.1174058825155740310 ) ) ;
#12893 = ORIENTED_EDGE ( 'NONE', *, *, #2449, .T. ) ;
#12894 = CARTESIAN_POINT ( 'NONE',  ( 0.2678247992155382007, 5.080760836019062587, 0.1601480313148006818 ) ) ;
#12895 = CARTESIAN_POINT ( 'NONE',  ( 0.2764156081756483641, 0.1144950937579610056, 0.2306944444444475328 ) ) ;
#12896 = CARTESIAN_POINT ( 'NONE',  ( -1.726321361862525858E-17, 4.227861111186976828, -0.2819296736111110979 ) ) ;
#12897 = CARTESIAN_POINT ( 'NONE',  ( -0.1993543840281266910, 5.123694444520309865, -0.1993543840281266910 ) ) ;
#12898 = CARTESIAN_POINT ( 'NONE',  ( 0.2353592251390298207, -0.1755526922479773988, 0.4047588300480876589 ) ) ;
#12899 = CARTESIAN_POINT ( 'NONE',  ( -0.2491998977626836975, 4.218580871723631276, -0.1921089702143923827 ) ) ;
#12900 = CARTESIAN_POINT ( 'NONE',  ( 0.1292346314604058410, 3.901472222222222008, 0.3119999999999998885 ) ) ;
#12901 = CARTESIAN_POINT ( 'NONE',  ( 0.3119999999999999996, 5.029944444596177178, -3.820898013339742174E-17 ) ) ;
#12902 = EDGE_CURVE ( 'NONE', #20713, #13860, #3644, .T. ) ;
#12903 = CARTESIAN_POINT ( 'NONE',  ( 0.2819296736111110979, 5.175777777853643791, -0.1167790944451423396 ) ) ;
#12904 = AXIS2_PLACEMENT_3D ( 'NONE', #7792, #11702, #20716 ) ;
#12905 = B_SPLINE_CURVE_WITH_KNOTS ( 'NONE', 3,
 ( #3894, #9504, #16938, #23484, #21318, #14241, #3024, #4841 ),
 .UNSPECIFIED., .F., .F.,
 ( 4, 2, 2, 4 ),
 ( 0.000000000000000000, 0.0004997454757086380699, 0.0007496182135629584058, 0.0009994909514172787418 ),
 .UNSPECIFIED. ) ;
#12906 = FACE_OUTER_BOUND ( 'NONE', #9411, .T. ) ;
#12907 = CARTESIAN_POINT ( 'NONE',  ( -0.2386252316775615556, 0.05573247922623769668, 0.1905836568333658665 ) ) ;
#12908 = CARTESIAN_POINT ( 'NONE',  ( -0.3155070326520293400, 0.1306872919485614903, 0.2289583333333365389 ) ) ;
#12909 = CARTESIAN_POINT ( 'NONE',  ( 0.1167790944451422702, 5.002166666742531298, -0.2819296736111110424 ) ) ;
#12910 = CARTESIAN_POINT ( 'NONE',  ( 0.4254812175019097586, -0.2956141819053919040, 0.4012599972958754702 ) ) ;
#12911 = ADVANCED_FACE ( 'NONE', ( #10977 ), #1997, .F. ) ;
#12912 = CARTESIAN_POINT ( 'NONE',  ( 0.3613381517857143232, 0.4187499999024575370, 0.1174058825155742114 ) ) ;
#12913 = ADVANCED_FACE ( 'NONE', ( #14389 ), #13264, .F. ) ;
#12914 = AXIS2_PLACEMENT_3D ( 'NONE', #4854, #21330, #2907 ) ;
#12915 = EDGE_CURVE ( 'NONE', #23182, #5345, #5826, .T. ) ;
#12916 = EDGE_LOOP ( 'NONE', ( #23691, #20057, #20026, #2208, #3220, #15317, #3102, #16729 ) ) ;
#12917 = CARTESIAN_POINT ( 'NONE',  ( -0.1993543840281266633, 0.2923611110352444808, -0.1993543840281266910 ) ) ;
#12918 = CARTESIAN_POINT ( 'NONE',  ( 0.2764156081756484196, -5.077672346800151106E-17, 0.2897222222222257115 ) ) ;
#12919 = CARTESIAN_POINT ( 'NONE',  ( 5.178964085587577574E-17, 4.936194444520309865, 0.2819296736111110979 ) ) ;
#12920 = CARTESIAN_POINT ( 'NONE',  ( 0.02020074157040065502, 4.487702955821844419, -0.3115091454018745210 ) ) ;
#12921 = ORIENTED_EDGE ( 'NONE', *, *, #22477, .T. ) ;
#12922 = CARTESIAN_POINT ( 'NONE',  ( -0.1167790944451423257, 4.953555555631421470, -0.2819296736111110424 ) ) ;
#12923 = FACE_OUTER_BOUND ( 'NONE', #7954, .T. ) ;
#12924 = CYLINDRICAL_SURFACE ( 'NONE', #22199, 0.3125000000000000000 ) ;
#12925 = DIRECTION ( 'NONE',  ( -0.8660254037844443697, 0.000000000000000000, 0.4999999999999902300 ) ) ;
#12926 = CARTESIAN_POINT ( 'NONE',  ( 0.000000000000000000, 0.3125000000000000000, 0.3244444444444480324 ) ) ;
#12927 = CARTESIAN_POINT ( 'NONE',  ( 0.1292346314604056190, 4.700083333333332725, -0.3119999999999999996 ) ) ;
#12928 = CARTESIAN_POINT ( 'NONE',  ( -0.2819296736111110424, 4.078555555631420582, 0.1167790944451424923 ) ) ;
#12929 = DIRECTION ( 'NONE',  ( -0.000000000000000000, -1.000000000000000000, -0.000000000000000000 ) ) ;
#12930 = EDGE_CURVE ( 'NONE', #10368, #16166, #799, .T. ) ;
#12931 =( BOUNDED_CURVE ( )  B_SPLINE_CURVE ( 2, ( #10540, #17973, #6264, #779, #6385, #13834, #12019, #19432, #17606, #897, #16389, #16506, #1858 ),
 .UNSPECIFIED., .F., .F. ) 
 B_SPLINE_CURVE_WITH_KNOTS ( ( 3, 2, 2, 2, 2, 2, 3 ),
 ( 0.3214285714285714524, 0.3285714285714285698, 0.3428571428571428603, 0.3571428571428571508, 0.3714285714285714413, 0.3857142857142857317, 0.3928571428571429047 ),
 .UNSPECIFIED. ) 
 CURVE ( )  GEOMETRIC_REPRESENTATION_ITEM ( )  RATIONAL_B_SPLINE_CURVE ( ( 0.9755282581475767101, 0.9755282581475768211, 1.000000000000000000, 0.9510565162951535312, 1.000000000000000000, 0.9510565162951535312, 1.000000000000000000, 0.9510565162951535312, 1.000000000000000000, 0.9510565162951535312, 1.000000000000000000, 0.9755282581475765991, 0.9755282581475767101 ) ) 
 REPRESENTATION_ITEM ( '' )  );
#12932 = CARTESIAN_POINT ( 'NONE',  ( 0.2963938556121599732, 4.032736175004294488, -0.09744095219179720047 ) ) ;
#12933 = DIRECTION ( 'NONE',  ( 0.000000000000000000, 0.000000000000000000, 1.000000000000000000 ) ) ;
#12934 = EDGE_LOOP ( 'NONE', ( #3194, #23403, #19088, #21065 ) ) ;
#12935 = DIRECTION ( 'NONE',  ( 0.000000000000000000, 0.000000000000000000, -1.000000000000000000 ) ) ;
#12936 = ORIENTED_EDGE ( 'NONE', *, *, #1301, .T. ) ;
#12937 = DIRECTION ( 'NONE',  ( -6.148297094540788948E-16, -1.493785812010397437E-17, -1.000000000000000000 ) ) ;
#12938 = DIRECTION ( 'NONE',  ( -0.000000000000000000, 1.000000000000000000, -0.000000000000000000 ) ) ;
#12939 = CARTESIAN_POINT ( 'NONE',  ( 0.2764156081756483641, 0.1144950937579610056, 0.1751388888888914530 ) ) ;
#12940 = B_SPLINE_CURVE_WITH_KNOTS ( 'NONE', 3,
 ( #7317, #12578, #5232, #1344, #7197, #18170, #10501, #5111, #22183, #23639, #9023, #8901, #3532, #19999, #10619, #6955, #3169, #23516, #14642, #20120, #12343, #16102, #7078, #1466, #3286, #18290, #14273, #14517, #14767, #9140, #12705, #16227, #3411, #14397, #10861, #10983, #18409, #16585, #17933, #19759, #1587, #16464 ),
 .UNSPECIFIED., .F., .F.,
 ( 4, 2, 2, 2, 2, 2, 2, 2, 2, 2, 2, 2, 2, 2, 2, 2, 2, 2, 2, 2, 4 ),
 ( 0.01713591359826903762, 0.01767127539367114447, 0.01820663718907325479, 0.01927736077987746849, 0.02034808437068168566, 0.02141880796148589935, 0.02195416975688800620, 0.02248953155229011652, 0.02356025514309433022, 0.02463097873389854045, 0.02570170232470275415, 0.02677242591550696785, 0.02784314950631118502, 0.02891387309711539871, 0.02998459668791961241, 0.03051995848332171926, 0.03105532027872382611, 0.03212604386952803981, 0.03266140566493014319, 0.03319676746033224657, 0.03426749105113646027 ),
 .UNSPECIFIED. ) ;
#12941 = DIRECTION ( 'NONE',  ( -0.000000000000000000, -1.000000000000000000, -0.000000000000000000 ) ) ;
#12942 = CARTESIAN_POINT ( 'NONE',  ( 1.020000000000000018, 0.05000000000000028727, -2.591000000000000192 ) ) ;
#12943 = CARTESIAN_POINT ( 'NONE',  ( -0.1144950937579609918, -0.2764156081756484196, 0.3834722222222265997 ) ) ;
#12944 = CARTESIAN_POINT ( 'NONE',  ( 0.2233192592356399164, 0.2151785713310289672, 0.3073725909049500604 ) ) ;
#12945 = CARTESIAN_POINT ( 'NONE',  ( 1.726321361862525858E-17, 0.2715277777019111660, -0.2819296736111110979 ) ) ;
#12946 = CARTESIAN_POINT ( 'NONE',  ( 0.02550031897004510079, 3.876477113958451515, -0.3109980661668607094 ) ) ;
#12947 = DIRECTION ( 'NONE',  ( -0.000000000000000000, -1.000000000000000000, -0.000000000000000000 ) ) ;
#12948 = DIRECTION ( 'NONE',  ( -0.000000000000000000, -1.000000000000000000, -0.000000000000000000 ) ) ;
#12949 = CARTESIAN_POINT ( 'NONE',  ( -0.2764156081756484196, -0.1144950937579609362, -0.1234722222222220528 ) ) ;
#12950 = ORIENTED_EDGE ( 'NONE', *, *, #13032, .T. ) ;
#12951 = VERTEX_POINT ( 'NONE', #6525 ) ;
#12952 = CARTESIAN_POINT ( 'NONE',  ( -0.2944222112592022600, 5.102614573065762826, -0.1009617277478159353 ) ) ;
#12953 = CARTESIAN_POINT ( 'NONE',  ( -1.910449006669871087E-17, 4.370222222222221120, -0.3119999999999999996 ) ) ;
#12954 = CARTESIAN_POINT ( 'NONE',  ( -0.2819296736111110979, 0.5666666665908001166, 0.1167790944451422425 ) ) ;
#12955 = CARTESIAN_POINT ( 'NONE',  ( 5.178964085587577574E-17, 3.880638888964754951, 0.2819296736111110979 ) ) ;
#12956 = CARTESIAN_POINT ( 'NONE',  ( -0.2233192592356399442, 0.2508928570453147211, -0.3073725909049500049 ) ) ;
#12957 = CARTESIAN_POINT ( 'NONE',  ( 0.1167790944451422702, 4.349388888964754507, -0.2819296736111110424 ) ) ;
#12958 = DIRECTION ( 'NONE',  ( -0.000000000000000000, 1.000000000000000000, -0.000000000000000000 ) ) ;
#12959 = CARTESIAN_POINT ( 'NONE',  ( -0.1292346314604044533, 4.595916666666665762, -0.3120000000000012763 ) ) ;
#12960 = ORIENTED_EDGE ( 'NONE', *, *, #9559, .T. ) ;
#12961 = CARTESIAN_POINT ( 'NONE',  ( -7.331754493858430024E-07, 4.349360015129621004, 0.3119999999981767358 ) ) ;
#12962 = CARTESIAN_POINT ( 'NONE',  ( -1.726321361862525858E-17, 4.950083333409199149, -0.2819296736111110979 ) ) ;
#12963 = CARTESIAN_POINT ( 'NONE',  ( -0.2969476826539968473, 5.154194855657474150, -0.05166938045060873175 ) ) ;
#12964 = B_SPLINE_CURVE_WITH_KNOTS ( 'NONE', 3,
 ( #16619, #15036, #384, #7824, #17098, #20870, #1980, #2095, #22333, #24039, #3809, #11255 ),
 .UNSPECIFIED., .F., .F.,
 ( 4, 2, 2, 2, 2, 4 ),
 ( 0.000000000000000000, 0.003350371137362711908, 0.006700742274725423817, 0.01005111341208813659, 0.01172629898076949471, 0.01340148454945085110 ),
 .UNSPECIFIED. ) ;
#12965 = CARTESIAN_POINT ( 'NONE',  ( 0.1993543840281267465, 4.651472222298087544, 0.1993543840281266633 ) ) ;
#12966 =( BOUNDED_CURVE ( )  B_SPLINE_CURVE ( 2, ( #23224, #6533, #13986, #21413, #6654, #23955, #18359, #16536, #10811, #18239, #20430, #16772, #5431, #8969, #3480, #9216, #16655, #1652, #3597, #9087, #13137, #7503, #5672, #7149, #12897, #1771, #3726, #14717, #18601, #11173, #14951, #7269, #7385, #14589, #20313, #3359, #22130, #1538, #5550, #11049, #24076, #12773, #10931, #13015, #18478, #20191, #14836, #22254, #1893, #9336, #56, #22370, #20550, #12653, #20071, #16418, #23827, #22012, #5310, #10764, #10287, #2954, #17711, #19779, #21606, #8673, #16125, #5014, #19899, #16002, #21730, #23658, #12362, #18067, #16247, #5134, #21845, #10411, #23420, #4899, #1487, #3079, #7101, #1005, #23539, #8924, #16369, #18191, #5256, #10522, #3188, #6731, #8435, #12480, #23778, #1246, #17953, #1369, #6854, #14539, #19656, #21487, #12598, #8795, #20144, #15880, #20018, #6976, #8561, #14296, #12243, #10636, #14419, #12726, #4774, #1127, #3307, #21962, #23297, #6609, #14057, #17836, #14174, #16606, #20502, #3797, #7336, #14900, #14788, #5859, #7452, #18550, #22204, #5746, #16959, #22570, #23899, #18789, #3917, #1839, #7574, #1967, #12845, #9282, #1609, #20381, #9043, #15022, #3673, #11241, #13318, #11120, #22321, #22446, #3550, #5503, #14664, #11361, #24026, #3430, #12965, #13204, #9406, #2084, #16844, #10883, #16489, #18312, #9526, #7218, #18668, #131, #11001, #16724, #20617, #254, #4, #5622, #7694, #13087, #1724, #15141, #22084, #5379, #20265, #18428, #9162, #12866, #20637, #393, #1862, #11504, #5400, #3819, #13337, #20759, #22591, #9668, #14923, #7594, #20402, #2236, #16979, #18447, #9425, #22466, #5524, #5644, #1989, #11380, #18687, #18808, #16864, #2104, #13108, #20285, #7474, #151, #17105, #7357, #14687, #4049, #5877, #22105, #22342, #15044, #3695, #3570, #9303, #11141, #20521, #18571, #11262, #9184, #18938, #1744, #9546, #22224, #14807, #273, #11023, #16628, #5766, #24047, #12988, #16744, #13226, #26, #3938, #7713, #15159, #22826, #19054, #19731, #15952, #18026, #22705, #3033, #23377, #6116, #17667, #14251, #6685, #3149, #4969, #953, #11747, #8384, #13461, #20878, #10480, #6809, #14014, #2355, #20997, #1079, #8511, #19168, #19609, #2786, #10598, #21686, #7832, #9796, #21444, #17787, #17912, #23254, #8636, #1205, #12436, #15836, #14130, #17229, #4730, #5995, #6563, #4172, #12318, #12202, #21559, #2904, #10363, #16081, #7943, #10239, #511, #23493, #4290, #15278, #4850, #19852, #11625, #15399, #13585, #14618, #9116, #12803, #16320, #19977, #3389, #22163, #1445, #10841, #7299, #12928, #18269, #7176, #14748, #20222, #23733, #9001, #1800, #5464, #23987, #16565, #16686, #20340, #23618, #3628, #11200, #18150, #8749, #1566, #12682, #23856, #22043, #3511, #10962, #7057, #18387, #11078, #16445, #18508, #9245, #24107, #7418, #8879, #5339, #1682, #14869, #20100, #22284, #16204, #5579, #13044, #20461, #3758, #1323, #6932, #14370, #14496, #21803, #5089, #21919, #12557, #5209, #3264, #10716, #22885, #5705, #22652, #22767, #5940, #6059, #17041, #16809, #11443, #4349, #3878, #8008, #9610, #9368, #2176, #16919, #13286, #9487, #13168, #13528, #2295, #18630, #22404, #13398, #334, #17170, #4112, #573, #456, #13642, #15460, #18876, #22527, #3992, #90, #7533, #20942, #17285, #7774, #20581, #7655, #11570, #15221, #20702, #2048, #18998, #9730, #6179, #21061, #11322 ),
 .UNSPECIFIED., .F., .T. ) 
 B_SPLINE_CURVE_WITH_KNOTS ( ( 3, 2, 2, 2, 2, 2, 2, 2, 2, 2, 2, 2, 2, 2, 2, 2, 2, 2, 2, 2, 2, 2, 2, 2, 2, 2, 2, 2, 2, 2, 2, 2, 2, 2, 2, 2, 2, 2, 2, 2, 2, 2, 2, 2, 2, 2, 2, 2, 2, 2, 2, 2, 2, 2, 2, 2, 2, 2, 2, 2, 2, 2, 2, 2, 2, 2, 2, 2, 2, 2, 2, 2, 2, 2, 2, 2, 2, 2, 2, 2, 2, 2, 2, 2, 2, 2, 2, 2, 2, 2, 2, 2, 2, 2, 2, 2, 2, 2, 2, 2, 2, 2, 2, 2, 2, 2, 2, 2, 2, 2, 2, 2, 2, 2, 2, 2, 2, 2, 2, 2, 2, 2, 2, 2, 2, 2, 2, 2, 2, 2, 2, 2, 2, 2, 2, 2, 2, 2, 2, 2, 2, 2, 2, 2, 2, 2, 2, 2, 2, 2, 2, 2, 2, 2, 2, 2, 2, 2, 2, 2, 2, 2, 2, 2, 2, 2, 2, 2, 2, 2, 2, 2, 2, 2, 2, 2, 2, 2, 2, 2, 2, 2, 2, 2, 2, 2, 2, 2, 2, 2, 2, 2, 2, 2, 2, 2, 2, 2, 2, 2, 2, 2, 2, 2, 2, 2, 2, 2, 2, 2, 2, 2, 2, 2, 3 ),
 ( 0.02311620385524515431, 0.02741254234740052656, 0.03198129940530199805, 0.03655005646320347301, 0.04111881352110494797, 0.04568757057900641599, 0.05025632763690789095, 0.05482508469480935898, 0.05939384175271084088, 0.06396259881061230890, 0.06853135586851377692, 0.07310011292641524494, 0.07766886998431671296, 0.08223762704221820874, 0.08680638410011967676, 0.09137514115802114478, 0.09594389821592259893, 0.1005126552738240808, 0.1050814123317255488, 0.1096501693896270169, 0.1142189264475284988, 0.1187876835054299807, 0.1233564405633314487, 0.1279251976212329167, 0.1324939546791343847, 0.1370627117370358805, 0.1416314687949373208, 0.1462002258528387888, 0.1507689829107402846, 0.1553377399686417248, 0.1599064970265432206, 0.1644752540844447164, 0.1690440111423461567, 0.1736127682002476524, 0.1781815252581490927, 0.1827502823160505885, 0.1873190393739520565, 0.1918877964318535245, 0.1964565534897550203, 0.2010253105476564883, 0.2055940676055579563, 0.2101628246634593966, 0.2147315817213608646, 0.2193003387792623327, 0.2238690958371638284, 0.2284378528950652965, 0.2330066099529667645, 0.2375753670108682603, 0.2421441240687697005, 0.2467128811266711963, 0.2512816381845726088, 0.2558503952424741046, 0.2604191523003756004, 0.2649879093582770961, 0.2695566664161785919, 0.2741254234740800322, 0.2786941805319814724, 0.2832629375898830237, 0.2878316946477844640, 0.2924004517056859043, 0.2969692087635873445, 0.3015379658214888403, 0.3061067228793902806, 0.3106754799372917208, 0.3152442369951933276, 0.3198129940530947679, 0.3243817511109962082, 0.3289505081688977040, 0.3335192652267991442, 0.3380880222847005845, 0.3426567793426020248, 0.3472255364005036316, 0.3517942934584050718, 0.3563630505163065121, 0.3609318075742080079, 0.3655005646321094481, 0.3700693216900108884, 0.3746380787479123842, 0.3792068358058139355, 0.3837755928637153757, 0.3883443499216168715, 0.3929131069795183118, 0.3974818640374197520, 0.4020506210953212478, 0.4066193781532226881, 0.4111881352111242394, 0.4157568922690256796, 0.4203256493269271754, 0.4248944063848286157, 0.4294631634427300004, 0.4340319205006314962, 0.4386006775585329365, 0.4431694346164344878, 0.4477381916743359835, 0.4523069487322374238, 0.4568757057901388641, 0.4614444628480403598, 0.4660132199059418001, 0.4705819769638432404, 0.4751507340217447917, 0.4797194910796462874, 0.4842882481375477277, 0.4888570051954491680, 0.4934257622533506638, 0.4979945193112521040, 0.5025632763691535443, 0.5071320334270551511, 0.5117007904849566469, 0.5162695475428580316, 0.5208383046007595274, 0.5254070616586609122, 0.5299758187165625190, 0.5345445757744640147, 0.5391133328323653995, 0.5436820898902668953, 0.5482508469481683910, 0.5528196040060697758, 0.5573883610639712716, 0.5619571181218727673, 0.5665258751797742631, 0.5710946322376757589, 0.5756633892955772547, 0.5802321463534786394, 0.5848009034113801352, 0.5893696604692815200, 0.5939384175271831268, 0.5985071745850845115, 0.6030759316429861183, 0.6076446887008875031, 0.6122134457587889989, 0.6167822028166903836, 0.6213509598745918794, 0.6259197169324933752, 0.6304884739903949820, 0.6350572310482963667, 0.6396259881061978625, 0.6441947451640992472, 0.6487635022220007430, 0.6533322592799021278, 0.6579010163378037346, 0.6624697733957052304, 0.6670385304536067261, 0.6716072875115081109, 0.6761760445694096067, 0.6807448016273109914, 0.6853135586852124872, 0.6898823157431140940, 0.6944510728010155898, 0.6990198298589169745, 0.7035885869168184703, 0.7081573439747198551, 0.7127261010326212398, 0.7172948580905228466, 0.7218636151484243424, 0.7264323722063258382, 0.7310011292642272229, 0.7355698863221287187, 0.7401386433800301035, 0.7447074004379315992, 0.7492761574958330950, 0.7538449145537347018, 0.7584136716116360866, 0.7629824286695375823, 0.7675511857274389671, 0.7721199427853404629, 0.7766886998432419587, 0.7812574569011434544, 0.7858262139590449502, 0.7903949710169464460, 0.7949637280748478307, 0.7995324851327493265, 0.8041012421906508223, 0.8086699992485523181, 0.8132387563064537028, 0.8178075133643553096, 0.8223762704222566944, 0.8269450274801581902, 0.8315137845380595749, 0.8360825415959611817, 0.8406512986538625665, 0.8452200557117640622, 0.8497888127696655580, 0.8543575698275670538, 0.8589263268854684386, 0.8634950839433700454, 0.8680638410012714301, 0.8726325980591729259, 0.8772013551170743106, 0.8817701121749759174, 0.8863388692328773022, 0.8909076262907786870, 0.8954763833486802938, 0.9000451404065816785, 0.9046138974644831743, 0.9091826545223845590, 0.9137514115802861658, 0.9183201686381875506, 0.9228889256960891574, 0.9274576827539905421, 0.9320264398118920379, 0.9365951968697934227, 0.9411639539276949185, 0.9457327109855964142, 0.9503014680434979100, 0.9548702251013994058, 0.9594389821593009016, 0.9640077392172022863, 0.9685764962751037821, 0.9731452533330051669, 0.9777140103909067737, 0.9822827674488082694, 0.9868515245067097652, 0.9914202815646111500, 0.9959890386225126457, 1.000000000000000000 ),
 .UNSPECIFIED. ) 
 CURVE ( )  GEOMETRIC_REPRESENTATION_ITEM ( )  RATIONAL_B_SPLINE_CURVE ( ( 0.9914636835865335840, 0.9284183224522696287, 1.000000000000000000, 0.9238795325112867385, 1.000000000000000000, 0.9238795325112867385, 1.000000000000000000, 0.9238795325112867385, 1.000000000000000000, 0.9238795325112867385, 1.000000000000000000, 0.9238795325112867385, 1.000000000000000000, 0.9238795325112867385, 1.000000000000000000, 0.9238795325112867385, 1.000000000000000000, 0.9238795325112867385, 1.000000000000000000, 0.9238795325112867385, 1.000000000000000000, 0.9238795325112867385, 1.000000000000000000, 0.9238795325112867385, 1.000000000000000000, 0.9238795325112867385, 1.000000000000000000, 0.9238795325112867385, 1.000000000000000000, 0.9238795325112867385, 1.000000000000000000, 0.9238795325112867385, 1.000000000000000000, 0.9238795325112867385, 1.000000000000000000, 0.9238795325112867385, 1.000000000000000000, 0.9238795325112867385, 1.000000000000000000, 0.9238795325112867385, 1.000000000000000000, 0.9238795325112867385, 1.000000000000000000, 0.9238795325112867385, 1.000000000000000000, 0.9238795325112867385, 1.000000000000000000, 0.9238795325112867385, 1.000000000000000000, 0.9238795325112867385, 1.000000000000000000, 0.9238795325112867385, 1.000000000000000000, 0.9238795325112867385, 1.000000000000000000, 0.9238795325112867385, 1.000000000000000000, 0.9238795325112867385, 1.000000000000000000, 0.9238795325112867385, 1.000000000000000000, 0.9238795325112867385, 1.000000000000000000, 0.9238795325112867385, 1.000000000000000000, 0.9238795325112867385, 1.000000000000000000, 0.9238795325112867385, 1.000000000000000000, 0.9238795325112867385, 1.000000000000000000, 0.9238795325112867385, 1.000000000000000000, 0.9238795325112867385, 1.000000000000000000, 0.9238795325112867385, 1.000000000000000000, 0.9238795325112867385, 1.000000000000000000, 0.9238795325112867385, 1.000000000000000000, 0.9238795325112867385, 1.000000000000000000, 0.9238795325112867385, 1.000000000000000000, 0.9238795325112867385, 1.000000000000000000, 0.9238795325112867385, 1.000000000000000000, 0.9238795325112867385, 1.000000000000000000, 0.9238795325112867385, 1.000000000000000000, 0.9238795325112867385, 1.000000000000000000, 0.9238795325112867385, 1.000000000000000000, 0.9238795325112867385, 1.000000000000000000, 0.9238795325112867385, 1.000000000000000000, 0.9238795325112867385, 1.000000000000000000, 0.9238795325112867385, 1.000000000000000000, 0.9238795325112867385, 1.000000000000000000, 0.9238795325112867385, 1.000000000000000000, 0.9238795325112867385, 1.000000000000000000, 0.9238795325112867385, 1.000000000000000000, 0.9238795325112867385, 1.000000000000000000, 0.9238795325112867385, 1.000000000000000000, 0.9238795325112867385, 1.000000000000000000, 0.9238795325112867385, 1.000000000000000000, 0.9238795325112867385, 1.000000000000000000, 0.9238795325112867385, 1.000000000000000000, 0.9238795325112867385, 1.000000000000000000, 0.9238795325112867385, 1.000000000000000000, 0.9238795325112867385, 1.000000000000000000, 0.9238795325112867385, 1.000000000000000000, 0.9238795325112867385, 1.000000000000000000, 0.9238795325112867385, 1.000000000000000000, 0.9238795325112867385, 1.000000000000000000, 0.9238795325112867385, 1.000000000000000000, 0.9238795325112867385, 1.000000000000000000, 0.9238795325112867385, 1.000000000000000000, 0.9238795325112867385, 1.000000000000000000, 0.9238795325112867385, 1.000000000000000000, 0.9238795325112867385, 1.000000000000000000, 0.9238795325112867385, 1.000000000000000000, 0.9238795325112867385, 1.000000000000000000, 0.9238795325112867385, 1.000000000000000000, 0.9238795325112867385, 1.000000000000000000, 0.9238795325112867385, 1.000000000000000000, 0.9238795325112867385, 1.000000000000000000, 0.9238795325112867385, 1.000000000000000000, 0.9238795325112867385, 1.000000000000000000, 0.9238795325112867385, 1.000000000000000000, 0.9238795325112867385, 1.000000000000000000, 0.9238795325112867385, 1.000000000000000000, 0.9238795325112867385, 1.000000000000000000, 0.9238795325112867385, 1.000000000000000000, 0.9238795325112867385, 1.000000000000000000, 0.9238795325112867385, 1.000000000000000000, 0.9238795325112867385, 1.000000000000000000, 0.9238795325112867385, 1.000000000000000000, 0.9238795325112867385, 1.000000000000000000, 0.9238795325112867385, 1.000000000000000000, 0.9238795325112867385, 1.000000000000000000, 0.9238795325112867385, 1.000000000000000000, 0.9238795325112867385, 1.000000000000000000, 0.9238795325112867385, 1.000000000000000000, 0.9238795325112867385, 1.000000000000000000, 0.9238795325112867385, 1.000000000000000000, 0.9238795325112867385, 1.000000000000000000, 0.9238795325112867385, 1.000000000000000000, 0.9238795325112867385, 1.000000000000000000, 0.9238795325112867385, 1.000000000000000000, 0.9238795325112867385, 1.000000000000000000, 0.9238795325112867385, 1.000000000000000000, 0.9238795325112867385, 1.000000000000000000, 0.9238795325112867385, 1.000000000000000000, 0.9238795325112867385, 1.000000000000000000, 0.9238795325112867385, 1.000000000000000000, 0.9238795325112867385, 1.000000000000000000, 0.9238795325112867385, 1.000000000000000000, 0.9238795325112867385, 1.000000000000000000, 0.9238795325112867385, 1.000000000000000000, 0.9238795325112867385, 1.000000000000000000, 0.9238795325112867385, 1.000000000000000000, 0.9238795325112867385, 1.000000000000000000, 0.9238795325112867385, 1.000000000000000000, 0.9238795325112867385, 1.000000000000000000, 0.9238795325112867385, 1.000000000000000000, 0.9238795325112867385, 1.000000000000000000, 0.9238795325112867385, 1.000000000000000000, 0.9238795325112867385, 1.000000000000000000, 0.9238795325112867385, 1.000000000000000000, 0.9238795325112867385, 1.000000000000000000, 0.9238795325112867385, 1.000000000000000000, 0.9238795325112867385, 1.000000000000000000, 0.9238795325112867385, 1.000000000000000000, 0.9238795325112867385, 1.000000000000000000, 0.9238795325112867385, 1.000000000000000000, 0.9238795325112867385, 1.000000000000000000, 0.9238795325112867385, 1.000000000000000000, 0.9238795325112867385, 1.000000000000000000, 0.9238795325112867385, 1.000000000000000000, 0.9238795325112867385, 1.000000000000000000, 0.9238795325112867385, 1.000000000000000000, 0.9238795325112867385, 1.000000000000000000, 0.9238795325112867385, 1.000000000000000000, 0.9238795325112867385, 1.000000000000000000, 0.9238795325112867385, 1.000000000000000000, 0.9238795325112867385, 1.000000000000000000, 0.9238795325112867385, 1.000000000000000000, 0.9238795325112867385, 1.000000000000000000, 0.9238795325112867385, 1.000000000000000000, 0.9238795325112867385, 1.000000000000000000, 0.9238795325112867385, 1.000000000000000000, 0.9238795325112867385, 1.000000000000000000, 0.9238795325112867385, 1.000000000000000000, 0.9238795325112867385, 1.000000000000000000, 0.9238795325112867385, 1.000000000000000000, 0.9238795325112867385, 1.000000000000000000, 0.9238795325112867385, 1.000000000000000000, 0.9238795325112867385, 1.000000000000000000, 0.9238795325112867385, 1.000000000000000000, 0.9238795325112867385, 1.000000000000000000, 0.9238795325112867385, 1.000000000000000000, 0.9238795325112867385, 1.000000000000000000, 0.9238795325112867385, 1.000000000000000000, 0.9238795325112867385, 1.000000000000000000, 0.9238795325112867385, 1.000000000000000000, 0.9238795325112867385, 1.000000000000000000, 0.9238795325112867385, 1.000000000000000000, 0.9238795325112867385, 1.000000000000000000, 0.9238795325112867385, 1.000000000000000000, 0.9238795325112867385, 1.000000000000000000, 0.9238795325112867385, 1.000000000000000000, 0.9238795325112867385, 1.000000000000000000, 0.9238795325112867385, 1.000000000000000000, 0.9238795325112867385, 1.000000000000000000, 0.9238795325112867385, 1.000000000000000000, 0.9238795325112867385, 1.000000000000000000, 0.9238795325112867385, 1.000000000000000000, 0.9238795325112867385, 1.000000000000000000, 0.9238795325112867385, 1.000000000000000000, 0.9238795325112867385, 1.000000000000000000, 0.9238795325112867385, 1.000000000000000000, 0.9238795325112867385, 1.000000000000000000, 0.9238795325112867385, 1.000000000000000000, 0.9238795325112867385, 1.000000000000000000, 0.9238795325112867385, 1.000000000000000000, 0.9238795325112867385, 1.000000000000000000, 0.9238795325112867385, 1.000000000000000000, 0.9238795325112867385, 1.000000000000000000, 0.9238795325112867385, 1.000000000000000000, 0.9238795325112867385, 1.000000000000000000, 0.9238795325112867385, 1.000000000000000000, 0.9238795325112867385, 1.000000000000000000, 0.9238795325112867385, 1.000000000000000000, 0.9238795325112867385, 1.000000000000000000, 0.9238795325112867385, 1.000000000000000000, 0.9238795325112867385, 1.000000000000000000, 0.9238795325112867385, 1.000000000000000000, 0.9238795325112867385, 1.000000000000000000, 0.9238795325112867385, 1.000000000000000000, 0.9238795325112867385, 1.000000000000000000, 0.9238795325112867385, 1.000000000000000000, 0.9238795325112867385, 1.000000000000000000, 0.9238795325112867385, 1.000000000000000000, 0.9238795325112867385, 1.000000000000000000, 0.9238795325112867385, 1.000000000000000000, 0.9238795325112867385, 1.000000000000000000, 0.9238795325112867385, 1.000000000000000000, 0.9238795325112867385, 1.000000000000000000, 0.9238795325112867385, 1.000000000000000000, 0.9238795325112867385, 1.000000000000000000, 0.9238795325112867385, 1.000000000000000000, 0.9238795325112867385, 1.000000000000000000, 0.9238795325112867385, 1.000000000000000000, 0.9238795325112867385, 1.000000000000000000, 0.9238795325112867385, 1.000000000000000000, 0.9238795325112867385, 1.000000000000000000, 0.9238795325112867385, 1.000000000000000000, 0.9238795325112867385, 1.000000000000000000, 0.9331730159288109672, 0.9836823002065551158 ) ) 
 REPRESENTATION_ITEM ( '' )  );
#12967 = CALENDAR_DATE ( 2026, 7, 10 ) ;
#12968 = CARTESIAN_POINT ( 'NONE',  ( 1.263940036315143372E-16, 0.9300000000000000488, -1.015181661097394050 ) ) ;
#12969 = CARTESIAN_POINT ( 'NONE',  ( -0.3119999999999999996, 0.4277777776260448528, -3.820898013339742174E-17 ) ) ;
#12970 = CARTESIAN_POINT ( 'NONE',  ( 0.2819296736111110424, 0.5527777777019112770, -0.1167790944451423119 ) ) ;
#12971 = VERTEX_POINT ( 'NONE', #19452 ) ;
#12972 = CARTESIAN_POINT ( 'NONE',  ( 1.726321361862525858E-17, 0.1743055554796889284, -0.2819296736111110979 ) ) ;
#12973 = CARTESIAN_POINT ( 'NONE',  ( -0.4749999999999999778, 3.700000000000000622, 2.908536147974962357E-17 ) ) ;
#12974 = CARTESIAN_POINT ( 'NONE',  ( 0.3003475124358241377, 0.9548081934128058723, 3.454202664143258605 ) ) ;
#12975 = CARTESIAN_POINT ( 'NONE',  ( -0.2472135954999579999, -0.05357142857142858927, 0.3402603233408159622 ) ) ;
#12976 = CARTESIAN_POINT ( 'NONE',  ( 0.3155070326520292290, -0.1306872919485616569, 0.03104166666666787963 ) ) ;
#12977 = VECTOR ( 'NONE', #12925, 39.37007874015747433 ) ;
#12978 = CARTESIAN_POINT ( 'NONE',  ( -0.4224968603155689340, -0.2973372013303092753, 0.07046346805499673072 ) ) ;
#12979 = CARTESIAN_POINT ( 'NONE',  ( -0.2546317497922950812, 3.885572683902586366, -0.1803043470822305872 ) ) ;
#12980 = CARTESIAN_POINT ( 'NONE',  ( 0.1167790944451423535, 0.2472222221463555580, 0.2819296736111110979 ) ) ;
#12981 = CARTESIAN_POINT ( 'NONE',  ( -0.2819296736111110424, 0.004166666590800034188, -0.1167790944451423396 ) ) ;
#12982 = CARTESIAN_POINT ( 'NONE',  ( -0.1167790944451423535, 4.432722222298088433, 0.2819296736111110424 ) ) ;
#12983 = VERTEX_POINT ( 'NONE', #8226 ) ;
#12984 = CARTESIAN_POINT ( 'NONE',  ( -7.726019084026502927E-17, 0.08749999980491522666, 0.4205848896953069405 ) ) ;
#12985 = CARTESIAN_POINT ( 'NONE',  ( 0.2631688084094599978, 4.535002051990153937, -0.1700533999623941861 ) ) ;
#12986 = CARTESIAN_POINT ( 'NONE',  ( 0.1167790944451422702, 5.071611111186976828, -0.2819296736111110424 ) ) ;
#12987 = ADVANCED_FACE ( 'NONE', ( #10201 ), #23095, .F. ) ;
#12988 = CARTESIAN_POINT ( 'NONE',  ( -0.1993543840281266355, 4.359805555631421470, 0.1993543840281267465 ) ) ;
#12989 = CARTESIAN_POINT ( 'NONE',  ( 0.2225846330532430251, 3.759095655877711106, -0.2199039815225819205 ) ) ;
#12990 = CARTESIAN_POINT ( 'NONE',  ( -0.3064624847683589115, 0.3533192024756441341, 0.4298724737630857384 ) ) ;
#12991 = CARTESIAN_POINT ( 'NONE',  ( -0.2977100099089716734, 3.659999999999999698, -0.09499999999999995948 ) ) ;
#12992 = CARTESIAN_POINT ( 'NONE',  ( -0.3119999999999999996, 4.113277777929510215, 0.000000000000000000 ) ) ;
#12993 = CARTESIAN_POINT ( 'NONE',  ( -0.1167790944451423535, 4.432722222298088433, 0.2819296736111110979 ) ) ;
#12994 = DIRECTION ( 'NONE',  ( 0.000000000000000000, -0.9659258262890682012, 0.2588190451025213501 ) ) ;
#12995 = ORIENTED_EDGE ( 'NONE', *, *, #5116, .F. ) ;
#12996 = ORIENTED_EDGE ( 'NONE', *, *, #776, .F. ) ;
#12997 = ORIENTED_EDGE ( 'NONE', *, *, #14198, .T. ) ;
#12998 = DATE_AND_TIME ( #18102, #11914 ) ;
#12999 = CARTESIAN_POINT ( 'NONE',  ( -0.2969103404914473776, -0.03343391069993188053, 0.4099802347466152130 ) ) ;
#13000 = CARTESIAN_POINT ( 'NONE',  ( 0.000000000000000000, 2.740000000000000213, -2.986000000000000210 ) ) ;
#13001 = CARTESIAN_POINT ( 'NONE',  ( -0.1166234456863257940, 4.111524471938507119, -2.802594437230254254 ) ) ;
#13002 = ORIENTED_EDGE ( 'NONE', *, *, #13931, .T. ) ;
#13003 = CARTESIAN_POINT ( 'NONE',  ( 0.3119999999999999996, 0.5666666665149336923, 0.000000000000000000 ) ) ;
#13004 = VERTEX_POINT ( 'NONE', #13857 ) ;
#13005 = CARTESIAN_POINT ( 'NONE',  ( 0.08808798601665612793, 3.066692553488282957, 3.256612888476066558 ) ) ;
#13006 = CARTESIAN_POINT ( 'NONE',  ( -0.04033405356528133034, 5.128963404656787795, 0.3049483761492560174 ) ) ;
#13007 = CARTESIAN_POINT ( 'NONE',  ( -0.2206173157302027954, 0.2611111111111107386, -0.2206173157302028232 ) ) ;
#13008 = CARTESIAN_POINT ( 'NONE',  ( -0.2206173157302027954, 0.4833333333333329485, -0.2206173157302028232 ) ) ;
#13009 = CARTESIAN_POINT ( 'NONE',  ( 0.2233192592356400275, 0.1651785713310290615, -0.3073725909049499494 ) ) ;
#13010 = ORIENTED_EDGE ( 'NONE', *, *, #18562, .F. ) ;
#13011 = CARTESIAN_POINT ( 'NONE',  ( 0.3118346153924759778, 5.085807044887113548, -0.005734882727686576101 ) ) ;
#13012 = CARTESIAN_POINT ( 'NONE',  ( 0.1954553509668046640, -0.1954553509668047195, 0.2758333333333367055 ) ) ;
#13013 = AXIS2_PLACEMENT_3D ( 'NONE', #4620, #23138, #4855 ) ;
#13014 = CARTESIAN_POINT ( 'NONE',  ( 0.1167790944451422702, 4.168833333409199149, -0.2819296736111110424 ) ) ;
#13015 = CARTESIAN_POINT ( 'NONE',  ( 0.1167790944451422702, 5.057722222298087544, -0.2819296736111110979 ) ) ;
#13016 = DIRECTION ( 'NONE',  ( 0.000000000000000000, 0.000000000000000000, -1.000000000000000000 ) ) ;
#13017 = CARTESIAN_POINT ( 'NONE',  ( -0.01848103877824625041, 0.5441716683897389606, 0.04413116910601661003 ) ) ;
#13018 = CARTESIAN_POINT ( 'NONE',  ( 5.731347020009612645E-17, 3.786888888888888527, 0.3119999999999999996 ) ) ;
#13019 = CARTESIAN_POINT ( 'NONE',  ( 5.731347020009612645E-17, 4.682722222373953969, 0.3119999999999999996 ) ) ;
#13020 = CARTESIAN_POINT ( 'NONE',  ( 0.2819296736111110979, 5.120222222298088433, -0.1167790944451423396 ) ) ;
#13021 = DIRECTION ( 'NONE',  ( 0.000000000000000000, -1.000000000000000000, 0.000000000000000000 ) ) ;
#13022 = ORIENTED_EDGE ( 'NONE', *, *, #13812, .T. ) ;
#13023 = CARTESIAN_POINT ( 'NONE',  ( 0.1116596296178199860, 0.2223214284738861402, -0.3436530038418508792 ) ) ;
#13024 = ADVANCED_FACE ( 'NONE', ( #4579 ), #15117, .F. ) ;
#13025 = CARTESIAN_POINT ( 'NONE',  ( 0.1416419608836146093, 0.04025187610558324247, -0.2530322881355697162 ) ) ;
#13026 = ADVANCED_FACE ( 'NONE', ( #916 ), #8345, .T. ) ;
#13027 = APPROVAL_DATE_TIME ( #8890, #10165 ) ;
#13028 = AXIS2_PLACEMENT_3D ( 'NONE', #21586, #1593, #3174 ) ;
#13029 = CARTESIAN_POINT ( 'NONE',  ( -0.3155070326520292845, 1.931923388228935888E-17, 0.1768750000000028078 ) ) ;
#13030 = CARTESIAN_POINT ( 'NONE',  ( -0.1993543840281266355, 5.137583333409198261, 0.1993543840281267465 ) ) ;
#13031 = CARTESIAN_POINT ( 'NONE',  ( -2.617362320975981593E-17, -0.5289902422706636020, 0.3941886329748526263 ) ) ;
#13032 = EDGE_CURVE ( 'NONE', #8464, #19892, #19569, .T. ) ;
#13033 = CARTESIAN_POINT ( 'NONE',  ( 0.3613381517857143232, 0.3508928570453146989, 0.000000000000000000 ) ) ;
#13034 = CARTESIAN_POINT ( 'NONE',  ( -0.1993543840281266633, 0.1812499999241333482, -0.1993543840281266910 ) ) ;
#13035 = CARTESIAN_POINT ( 'NONE',  ( -0.1144950937579609918, -0.2764156081756484196, 0.2723611111111143845 ) ) ;
#13036 = CARTESIAN_POINT ( 'NONE',  ( 0.1993543840281266633, 4.901472222298088433, -0.1993543840281266910 ) ) ;
#13037 = CARTESIAN_POINT ( 'NONE',  ( 0.04820796449995154442, 5.072973651020436847, 0.3082531300064171864 ) ) ;
#13038 = CARTESIAN_POINT ( 'NONE',  ( -0.2819296736111110979, 4.908416666742532186, 0.000000000000000000 ) ) ;
#13039 = CARTESIAN_POINT ( 'NONE',  ( -0.3236067977499790249, 0.07678571409062948105, 0.2351141009169892271 ) ) ;
#13040 = CARTESIAN_POINT ( 'NONE',  ( 0.2730879860166738338, 4.111524471938507119, -3.027594437230249902 ) ) ;
#13041 = DIRECTION ( 'NONE',  ( -1.000000000000000000, 0.000000000000000000, 0.000000000000000000 ) ) ;
#13042 = CARTESIAN_POINT ( 'NONE',  ( 0.1357687531234556544, 0.06249999999999967387, 0.2838640674724194901 ) ) ;
#13043 = CARTESIAN_POINT ( 'NONE',  ( 0.3119999999999999996, 4.578555555555555046, -3.820898013339742174E-17 ) ) ;
#13044 = CARTESIAN_POINT ( 'NONE',  ( 0.2819296736111110979, 3.939666666742531742, -0.1167790944451423396 ) ) ;
#13045 = VECTOR ( 'NONE', #22279, 39.37007874015748854 ) ;
#13046 = DIRECTION ( 'NONE',  ( 0.000000000000000000, 0.000000000000000000, -1.000000000000000000 ) ) ;
#13047 = CARTESIAN_POINT ( 'NONE',  ( 0.3127134533877636846, 4.029674673160470455, 0.009354555642908121346 ) ) ;
#13048 = DIRECTION ( 'NONE',  ( -0.000000000000000000, 0.9961946980917454342, -0.08715574274765824914 ) ) ;
#13049 = CARTESIAN_POINT ( 'NONE',  ( -0.1060554323913378977, 1.041821957232212270, -2.874935959385435336 ) ) ;
#13050 = EDGE_LOOP ( 'NONE', ( #6843, #13371, #21521, #19644 ) ) ;
#13051 = EDGE_CURVE ( 'NONE', #10504, #14830, #8050, .T. ) ;
#13052 = CARTESIAN_POINT ( 'NONE',  ( -0.2077028099651906379, 4.120735818351255020, 0.2358420112239252020 ) ) ;
#13053 = ADVANCED_FACE ( 'NONE', ( #5173 ), #10675, .T. ) ;
#13054 = CARTESIAN_POINT ( 'NONE',  ( -0.2764156081756484196, 1.692557448933383907E-17, 0.1994444444444472553 ) ) ;
#13055 = AXIS2_PLACEMENT_3D ( 'NONE', #2216, #11480, #6218 ) ;
#13056 = DIRECTION ( 'NONE',  ( 0.8660254037844433705, -9.889024645172693219E-32, -0.4999999999999916733 ) ) ;
#13057 = EDGE_CURVE ( 'NONE', #7051, #20991, #3469, .T. ) ;
#13058 = CARTESIAN_POINT ( 'NONE',  ( 0.4805456235326253656, 0.2624941757204518611, 0.04270874187135768885 ) ) ;
#13059 = CARTESIAN_POINT ( 'NONE',  ( -0.3613381517857143232, 0.2616071427596003973, -4.425116109941954795E-17 ) ) ;
#13060 = CARTESIAN_POINT ( 'NONE',  ( -5.178964085587577574E-17, 0.2437499999241333204, 0.2819296736111110979 ) ) ;
#13061 = CARTESIAN_POINT ( 'NONE',  ( 0.05085440012827255329, 3.875780013435167426, -0.3079968891009477461 ) ) ;
#13062 = CARTESIAN_POINT ( 'NONE',  ( 0.000000000000000000, 6.000000000000000888, 0.000000000000000000 ) ) ;
#13063 = DIRECTION ( 'NONE',  ( 0.8660254037844434816, -0.000000000000000000, -0.4999999999999915068 ) ) ;
#13064 = CARTESIAN_POINT ( 'NONE',  ( 0.1144950937579609085, -0.2764156081756484751, 0.001527777777778949230 ) ) ;
#13065 =( BOUNDED_CURVE ( )  B_SPLINE_CURVE ( 2, ( #2663, #10113, #14239, #3022, #942, #4719, #13888, #12192, #19719, #831, #6434, #2775, #17898, #8259, #4606, #8372, #15939, #6551, #14001, #15823, #1193, #8625, #2891, #16070, #10351, #15709, #21674, #17775, #23607, #8499, #4959, #12426, #23123, #3139, #1313, #8737, #16193, #6921, #12068, #19482, #79, #18376, #3746, #11190, #13034, #7524, #5327, #22152, #10830, #3253, #16434, #18258, #12792, #1553, #20211, #23722, #9356, #16309, #9233, #12668, #21907, #16672, #3499, #10704, #22030, #14971, #23844, #1790, #1671, #20450, #10949, #3377, #7164, #20088, #7047, #24097, #12917, #5078, #19966, #7406, #20328, #3617, #14737, #18619, #11067, #12546, #1911, #9103, #8991, #18496, #14607, #23975, #16798, #18139, #1436, #8868, #14483, #5449, #14857, #16553, #7285, #22274, #5569, #5197, #17393, #20810, #2037, #20571, #9476, #13387, #22872, #17275, #19214, #7763, #20929, #7645, #4099, #3868, #15207, #11309, #2404, #22756, #8110, #22642, #17155, #560, #22516, #2165, #16909, #6167, #11432, #686, #5927, #4222, #15093, #11558, #9844, #6047, #13514, #13273, #20690, #22393, #11675, #19098, #5809, #18985, #7997, #15449, #2285, #9719, #13630, #445, #3981, #7876, #21048, #4338, #11789, #2521, #9963, #15326, #5694, #13157, #18742, #204, #18863, #9598, #17030, #324, #6772, #804, #12404 ),
 .UNSPECIFIED., .F., .F. ) 
 B_SPLINE_CURVE_WITH_KNOTS ( ( 3, 2, 2, 2, 2, 2, 2, 2, 2, 2, 2, 2, 2, 2, 2, 2, 2, 2, 2, 2, 2, 2, 2, 2, 2, 2, 2, 2, 2, 2, 2, 2, 2, 2, 2, 2, 2, 2, 2, 2, 2, 2, 2, 2, 2, 2, 2, 2, 2, 2, 2, 2, 2, 2, 2, 2, 2, 2, 2, 2, 2, 2, 2, 2, 2, 2, 2, 2, 2, 2, 2, 2, 2, 2, 2, 2, 2, 2, 2, 2, 2, 2, 2, 2, 2, 3 ),
 ( 0.05799230993249919475, 0.06250000000000000000, 0.07291666666666667129, 0.08333333333333332871, 0.09375000000000000000, 0.1041666666666666713, 0.1145833333333333287, 0.1250000000000000000, 0.1354166666666666574, 0.1458333333333333426, 0.1562500000000000000, 0.1666666666666666574, 0.1770833333333333426, 0.1875000000000000000, 0.1979166666666666852, 0.2083333333333333703, 0.2187500000000000000, 0.2291666666666666852, 0.2395833333333333703, 0.2500000000000000000, 0.2604166666666666852, 0.2708333333333333148, 0.2812500000000000000, 0.2916666666666666852, 0.3020833333333333148, 0.3125000000000000000, 0.3229166666666666852, 0.3333333333333333148, 0.3437500000000000000, 0.3541666666666666852, 0.3645833333333333148, 0.3750000000000000000, 0.3854166666666666852, 0.3958333333333333148, 0.4062500000000000000, 0.4166666666666666852, 0.4270833333333333148, 0.4375000000000000000, 0.4479166666666666852, 0.4583333333333333148, 0.4687500000000000000, 0.4791666666666666852, 0.4895833333333333148, 0.5000000000000000000, 0.5104166666666666297, 0.5208333333333333703, 0.5312500000000000000, 0.5416666666666666297, 0.5520833333333333703, 0.5625000000000000000, 0.5729166666666666297, 0.5833333333333333703, 0.5937500000000000000, 0.6041666666666666297, 0.6145833333333333703, 0.6250000000000000000, 0.6354166666666666297, 0.6458333333333333703, 0.6562500000000000000, 0.6666666666666666297, 0.6770833333333333703, 0.6875000000000000000, 0.6979166666666666297, 0.7083333333333333703, 0.7187500000000000000, 0.7291666666666666297, 0.7395833333333333703, 0.7500000000000000000, 0.7604166666666666297, 0.7708333333333333703, 0.7812500000000000000, 0.7916666666666666297, 0.8020833333333333703, 0.8125000000000000000, 0.8229166666666666297, 0.8333333333333333703, 0.8437500000000000000, 0.8541666666666666297, 0.8645833333333333703, 0.8750000000000000000, 0.8854166666666666297, 0.8958333333333333703, 0.9062500000000000000, 0.9166666666666666297, 0.9270833333333333703, 0.9375000000000000000 ),
 .UNSPECIFIED. ) 
 CURVE ( )  GEOMETRIC_REPRESENTATION_ITEM ( )  RATIONAL_B_SPLINE_CURVE ( ( 0.9626285260900115937, 0.9670597623776904239, 1.000000000000000000, 0.9238795325112867385, 1.000000000000000000, 0.9238795325112867385, 1.000000000000000000, 0.9238795325112867385, 1.000000000000000000, 0.9238795325112867385, 1.000000000000000000, 0.9238795325112867385, 1.000000000000000000, 0.9238795325112867385, 1.000000000000000000, 0.9238795325112867385, 1.000000000000000000, 0.9238795325112867385, 1.000000000000000000, 0.9238795325112867385, 1.000000000000000000, 0.9238795325112867385, 1.000000000000000000, 0.9238795325112867385, 1.000000000000000000, 0.9238795325112867385, 1.000000000000000000, 0.9238795325112867385, 1.000000000000000000, 0.9238795325112867385, 1.000000000000000000, 0.9238795325112867385, 1.000000000000000000, 0.9238795325112867385, 1.000000000000000000, 0.9238795325112867385, 1.000000000000000000, 0.9238795325112867385, 1.000000000000000000, 0.9238795325112867385, 1.000000000000000000, 0.9238795325112867385, 1.000000000000000000, 0.9238795325112867385, 1.000000000000000000, 0.9238795325112867385, 1.000000000000000000, 0.9238795325112867385, 1.000000000000000000, 0.9238795325112867385, 1.000000000000000000, 0.9238795325112867385, 1.000000000000000000, 0.9238795325112867385, 1.000000000000000000, 0.9238795325112867385, 1.000000000000000000, 0.9238795325112867385, 1.000000000000000000, 0.9238795325112867385, 1.000000000000000000, 0.9238795325112867385, 1.000000000000000000, 0.9238795325112867385, 1.000000000000000000, 0.9238795325112867385, 1.000000000000000000, 0.9238795325112867385, 1.000000000000000000, 0.9238795325112867385, 1.000000000000000000, 0.9238795325112867385, 1.000000000000000000, 0.9238795325112867385, 1.000000000000000000, 0.9238795325112867385, 1.000000000000000000, 0.9238795325112867385, 1.000000000000000000, 0.9238795325112867385, 1.000000000000000000, 0.9238795325112867385, 1.000000000000000000, 0.9238795325112867385, 1.000000000000000000, 0.9238795325112867385, 1.000000000000000000, 0.9238795325112867385, 1.000000000000000000, 0.9238795325112867385, 1.000000000000000000, 0.9238795325112867385, 1.000000000000000000, 0.9238795325112867385, 1.000000000000000000, 0.9238795325112867385, 1.000000000000000000, 0.9238795325112867385, 1.000000000000000000, 0.9238795325112867385, 1.000000000000000000, 0.9238795325112867385, 1.000000000000000000, 0.9238795325112867385, 1.000000000000000000, 0.9238795325112867385, 1.000000000000000000, 0.9238795325112867385, 1.000000000000000000, 0.9238795325112867385, 1.000000000000000000, 0.9238795325112867385, 1.000000000000000000, 0.9238795325112867385, 1.000000000000000000, 0.9238795325112867385, 1.000000000000000000, 0.9238795325112867385, 1.000000000000000000, 0.9238795325112867385, 1.000000000000000000, 0.9238795325112867385, 1.000000000000000000, 0.9238795325112867385, 1.000000000000000000, 0.9238795325112867385, 1.000000000000000000, 0.9238795325112867385, 1.000000000000000000, 0.9238795325112867385, 1.000000000000000000, 0.9238795325112867385, 1.000000000000000000, 0.9238795325112867385, 1.000000000000000000, 0.9238795325112867385, 1.000000000000000000, 0.9238795325112867385, 1.000000000000000000, 0.9238795325112867385, 1.000000000000000000, 0.9238795325112867385, 1.000000000000000000, 0.9238795325112867385, 1.000000000000000000, 0.9238795325112867385, 1.000000000000000000, 0.9238795325112867385, 1.000000000000000000, 0.9238795325112867385, 1.000000000000000000, 0.9238795325112867385, 1.000000000000000000, 0.9238795325112867385, 1.000000000000000000, 0.9238795325112867385, 1.000000000000000000, 0.9238795325112867385, 1.000000000000000000, 0.9238795325112867385, 1.000000000000000000, 0.9238795325112867385, 1.000000000000000000, 0.9238795325112867385, 1.000000000000000000, 0.9238795325112867385, 1.000000000000000000, 0.9238795325112867385, 1.000000000000000000, 0.9238795325112867385, 1.000000000000000000 ) ) 
 REPRESENTATION_ITEM ( '' )  );
#13066 = DIRECTION ( 'NONE',  ( -0.000000000000000000, 1.000000000000000000, -0.000000000000000000 ) ) ;
#13067 =( BOUNDED_CURVE ( )  B_SPLINE_CURVE ( 2, ( #15031, #22578, #20511, #6105, #13097, #5985, #9415, #18676, #19043, #4280, #20747, #1848, #18926 ),
 .UNSPECIFIED., .F., .F. ) 
 B_SPLINE_CURVE_WITH_KNOTS ( ( 3, 2, 2, 2, 2, 2, 3 ),
 ( 0.7500000000000000000, 0.7571428571428571175, 0.7714285714285714635, 0.7857142857142856984, 0.8000000000000000444, 0.8142857142857142794, 0.8214285714285715079 ),
 .UNSPECIFIED. ) 
 CURVE ( )  GEOMETRIC_REPRESENTATION_ITEM ( )  RATIONAL_B_SPLINE_CURVE ( ( 0.9755282581475768211, 0.9755282581475768211, 1.000000000000000000, 0.9510565162951535312, 1.000000000000000000, 0.9510565162951535312, 1.000000000000000000, 0.9510565162951535312, 1.000000000000000000, 0.9510565162951535312, 1.000000000000000000, 0.9755282581475765991, 0.9755282581475768211 ) ) 
 REPRESENTATION_ITEM ( '' )  );
#13068 = CARTESIAN_POINT ( 'NONE',  ( 0.2206173157302027954, 4.363277777777777366, -0.2206173157302028232 ) ) ;
#13069 = AXIS2_PLACEMENT_3D ( 'NONE', #20379, #9280, #1 ) ;
#13070 = CARTESIAN_POINT ( 'NONE',  ( 0.3119999999999999996, 0.07361111111111078020, 0.000000000000000000 ) ) ;
#13071 = CARTESIAN_POINT ( 'NONE',  ( 0.3119999999999999996, 5.075083333333332725, 0.1292346314604056190 ) ) ;
#13072 = CARTESIAN_POINT ( 'NONE',  ( 0.1116596296178199027, 0.2830357141881718053, 0.3436530038418508792 ) ) ;
#13073 = CARTESIAN_POINT ( 'NONE',  ( -0.1993543840281266355, 4.151472222298088433, 0.1993543840281267465 ) ) ;
#13074 = DIRECTION ( 'NONE',  ( -0.000000000000000000, -1.000000000000000000, -0.000000000000000000 ) ) ;
#13075 = EDGE_CURVE ( 'NONE', #18643, #11465, #4933, .T. ) ;
#13076 = DIRECTION ( 'NONE',  ( 1.707404996040164512E-16, 0.000000000000000000, -1.000000000000000000 ) ) ;
#13077 = ORIENTED_EDGE ( 'NONE', *, *, #23286, .F. ) ;
#13078 = CARTESIAN_POINT ( 'NONE',  ( -0.1993543840281266910, 4.845916666742532186, -0.1993543840281266910 ) ) ;
#13079 = VECTOR ( 'NONE', #18761, 39.37007874015748854 ) ;
#13080 = EDGE_CURVE ( 'NONE', #5177, #6611, #17404, .T. ) ;
#13081 = CARTESIAN_POINT ( 'NONE',  ( 0.000000000000000000, 0.000000000000000000, 0.000000000000000000 ) ) ;
#13082 = EDGE_CURVE ( 'NONE', #8012, #18459, #17871, .T. ) ;
#13083 = EDGE_CURVE ( 'NONE', #6253, #11779, #19907, .T. ) ;
#13084 = CARTESIAN_POINT ( 'NONE',  ( 0.003929474433554183514, 3.710394323774880654, -0.3119787920919602220 ) ) ;
#13085 = CARTESIAN_POINT ( 'NONE',  ( -0.1292346314604118085, 4.984805555555555934, -0.3119999999999938378 ) ) ;
#13086 = LOCAL_TIME ( 21, 9, 13.00000000000000000, #3341 ) ;
#13087 = CARTESIAN_POINT ( 'NONE',  ( -0.1167790944451423535, 4.585500000075865223, 0.2819296736111110979 ) ) ;
#13088 = DATE_TIME_ROLE ( 'classification_date' ) ;
#13089 = ADVANCED_FACE ( 'NONE', ( #8603 ), #3713, .T. ) ;
#13090 = FACE_OUTER_BOUND ( 'NONE', #1901, .T. ) ;
#13091 = DIRECTION ( 'NONE',  ( 0.000000000000000000, 1.000000000000000000, 0.000000000000000000 ) ) ;
#13092 = CARTESIAN_POINT ( 'NONE',  ( -0.1993543840281267465, 0.5284722221463555858, 0.1993543840281266633 ) ) ;
#13093 = ORIENTED_EDGE ( 'NONE', *, *, #14388, .F. ) ;
#13094 = ORIENTED_EDGE ( 'NONE', *, *, #13533, .T. ) ;
#13095 = CARTESIAN_POINT ( 'NONE',  ( -5.178964085587577574E-17, 0.2576388888130222155, 0.2819296736111110979 ) ) ;
#13096 = CARTESIAN_POINT ( 'NONE',  ( -0.003672251724678134415, 4.710598665704982757, -0.3119999984746245070 ) ) ;
#13097 = CARTESIAN_POINT ( 'NONE',  ( -0.3236067977499789694, 0.3482142855192008613, -0.2351141009169893104 ) ) ;
#13098 = VECTOR ( 'NONE', #984, 39.37007874015748143 ) ;
#13099 = CARTESIAN_POINT ( 'NONE',  ( 0.2472135954999579166, 0.1035714285714285227, 0.3402603233408160732 ) ) ;
#13100 = CARTESIAN_POINT ( 'NONE',  ( -3.863846776457871776E-17, -0.3155070326520292845, -0.03493055555555487496 ) ) ;
#13101 = DIRECTION ( 'NONE',  ( 0.4999999999999909517, -0.000000000000000000, -0.8660254037844438146 ) ) ;
#13102 = DIRECTION ( 'NONE',  ( -1.000000000000000000, 0.000000000000000000, 0.000000000000000000 ) ) ;
#13103 = CARTESIAN_POINT ( 'NONE',  ( -0.1167790944451424506, 0.3513888888130222155, 0.2819296736111110424 ) ) ;
#13104 = LINE ( 'NONE', #18442, #11998 ) ;
#13105 = CARTESIAN_POINT ( 'NONE',  ( 0.2819296736111110979, 4.283416666742533074, -3.452642723725051716E-17 ) ) ;
#13106 = CARTESIAN_POINT ( 'NONE',  ( 0.3999999999999999667, 0.1089285712334866069, -0.1299678784931625475 ) ) ;
#13107 = CARTESIAN_POINT ( 'NONE',  ( 5.178964085587577574E-17, 5.158416666742532186, 0.2819296736111110979 ) ) ;
#13108 = CARTESIAN_POINT ( 'NONE',  ( -0.2819296736111110979, 4.463972222298087544, 0.000000000000000000 ) ) ;
#13109 = CARTESIAN_POINT ( 'NONE',  ( 0.04095097312172040621, 4.931542214948650305, -0.3099778603826239265 ) ) ;
#13110 = LOCAL_TIME ( 21, 9, 13.00000000000000000, #18821 ) ;
#13111 = CARTESIAN_POINT ( 'NONE',  ( -0.3103970466387204197, 0.3620580589327443422, 0.08855978515309881338 ) ) ;
#13112 = CARTESIAN_POINT ( 'NONE',  ( -0.2206173157302027676, 4.009111111262843252, 0.2206173157302028787 ) ) ;
#13113 = LINE ( 'NONE', #18694, #551 ) ;
#13114 = APPLICATION_CONTEXT ( 'configuration controlled 3d designs of mechanical parts and assemblies' ) ;
#13115 = CARTESIAN_POINT ( 'NONE',  ( 0.2144047338281417914, -0.2134821532158128754, -0.09126195324992800173 ) ) ;
#13116 = ORIENTED_EDGE ( 'NONE', *, *, #21874, .F. ) ;
#13117 = VERTEX_POINT ( 'NONE', #22484 ) ;
#13118 = PERSON_AND_ORGANIZATION_ROLE ( 'creator' ) ;
#13119 = CARTESIAN_POINT ( 'NONE',  ( -0.2879402880768345274, -0.08326397218408013168, 0.4109361999077702499 ) ) ;
#13120 = EDGE_CURVE ( 'NONE', #5165, #13148, #9563, .T. ) ;
#13121 = CARTESIAN_POINT ( 'NONE',  ( -0.1363718491207122907, 4.845375667118064555, 0.2806196265496272435 ) ) ;
#13122 = DIRECTION ( 'NONE',  ( 0.000000000000000000, -0.7071067811865475727, 0.7071067811865475727 ) ) ;
#13123 = ORIENTED_EDGE ( 'NONE', *, *, #11553, .T. ) ;
#13124 = CARTESIAN_POINT ( 'NONE',  ( -0.2206173157302027954, 0.5874999998482670627, -0.2206173157302028232 ) ) ;
#13125 = VERTEX_POINT ( 'NONE', #5896 ) ;
#13126 = LINE ( 'NONE', #2122, #23785 ) ;
#13127 = CARTESIAN_POINT ( 'NONE',  ( 9.429780353434637026E-17, 0.9300000000000000488, -0.7700000000000013500 ) ) ;
#13128 = CARTESIAN_POINT ( 'NONE',  ( -0.3613381517857143232, 0.1008928570453147405, -4.425116109941954795E-17 ) ) ;
#13129 = CARTESIAN_POINT ( 'NONE',  ( -0.3125000000000000000, 0.000000000000000000, 1.326383476483184332 ) ) ;
#13130 = ORIENTED_EDGE ( 'NONE', *, *, #15111, .T. ) ;
#13131 = CARTESIAN_POINT ( 'NONE',  ( -0.2233192592356399442, 0.1080357141881718996, -0.3073725909049499494 ) ) ;
#13132 = CIRCLE ( 'NONE', #2599, 0.01875000000000000625 ) ;
#13133 = VERTEX_POINT ( 'NONE', #1760 ) ;
#13134 = CARTESIAN_POINT ( 'NONE',  ( 0.2573919081827345523, 5.080198807860221599, 0.1764520568086606067 ) ) ;
#13135 = CARTESIAN_POINT ( 'NONE',  ( -0.3104533523723745359, 4.669988699611968386, 0.03789925079919458095 ) ) ;
#13136 = CARTESIAN_POINT ( 'NONE',  ( 5.178964085587577574E-17, 4.255638888964754507, 0.2819296736111110979 ) ) ;
#13137 = CARTESIAN_POINT ( 'NONE',  ( -0.1993543840281266355, 5.137583333409198261, 0.1993543840281267465 ) ) ;
#13138 = CARTESIAN_POINT ( 'NONE',  ( -0.4687500000000003886, -0.04388698013647557988, 0.09139229829490845558 ) ) ;
#13139 = DIRECTION ( 'NONE',  ( 1.000000000000000000, 0.000000000000000000, -0.000000000000000000 ) ) ;
#13140 = CARTESIAN_POINT ( 'NONE',  ( 0.1292346314604056190, 3.866749999999999243, -0.3119999999999999996 ) ) ;
#13141 = CARTESIAN_POINT ( 'NONE',  ( -0.1292346314604056745, 4.658416666818398610, -0.3119999999999999996 ) ) ;
#13142 = CARTESIAN_POINT ( 'NONE',  ( 0.2819296736111111534, 5.168833333409199149, 0.1167790944451422563 ) ) ;
#13143 = DIRECTION ( 'NONE',  ( -0.3535533905932761733, -0.7071067811865487940, 0.6123724356957918058 ) ) ;
#13144 = CARTESIAN_POINT ( 'NONE',  ( 0.2923287055106771337, 0.05803571418817188299, 0.2123892367102621359 ) ) ;
#13145 = CC_DESIGN_PERSON_AND_ORGANIZATION_ASSIGNMENT ( #15439, #15198, ( #10901 ) ) ;
#13146 = LINE ( 'NONE', #69, #190 ) ;
#13147 = VECTOR ( 'NONE', #12947, 39.37007874015748143 ) ;
#13148 = VERTEX_POINT ( 'NONE', #9323 ) ;
#13149 = DATE_AND_TIME ( #3273, #9942 ) ;
#13150 = CARTESIAN_POINT ( 'NONE',  ( -0.1306872919485614903, 0.3155070326520293400, 0.3886805555555600256 ) ) ;
#13151 = CARTESIAN_POINT ( 'NONE',  ( -0.2819296736111110979, 5.130638888964754507, 0.000000000000000000 ) ) ;
#13152 = CARTESIAN_POINT ( 'NONE',  ( -0.1993543840281266355, 3.818138888964754507, 0.1993543840281267465 ) ) ;
#13153 = CARTESIAN_POINT ( 'NONE',  ( 0.02036138964301281717, 4.405474440628344368, 0.3119999972693427437 ) ) ;
#13154 = LINE ( 'NONE', #14605, #19590 ) ;
#13155 = DIRECTION ( 'NONE',  ( -1.000000000000000000, -0.000000000000000000, -0.000000000000000000 ) ) ;
#13156 = CARTESIAN_POINT ( 'NONE',  ( 0.1954553509668047195, 0.1954553509668046085, 0.1230555555555576941 ) ) ;
#13157 = CARTESIAN_POINT ( 'NONE',  ( -0.1167790944451424506, 0.5874999999241332649, 0.2819296736111110424 ) ) ;
#13158 = CARTESIAN_POINT ( 'NONE',  ( -0.2764156081756484196, 0.1144950937579609918, 0.3140277777777814583 ) ) ;
#13159 = CARTESIAN_POINT ( 'NONE',  ( -1.726321361862525858E-17, 4.963972222298088433, -0.2819296736111110979 ) ) ;
#13160 = CARTESIAN_POINT ( 'NONE',  ( 0.008437752171426261827, -0.5369270166837818437, 0.04763592618480781693 ) ) ;
#13161 = CARTESIAN_POINT ( 'NONE',  ( 0.1993543840281267465, 4.873694444520309865, 0.1993543840281266633 ) ) ;
#13162 = CARTESIAN_POINT ( 'NONE',  ( -0.1236067977499789583, 0.05535714266205805228, -0.3804226065180614791 ) ) ;
#13163 = CARTESIAN_POINT ( 'NONE',  ( 2.268515911781130585E-06, 4.877166605860494109, -0.3120000000014063746 ) ) ;
#13164 = CARTESIAN_POINT ( 'NONE',  ( -1.910449006669871087E-17, 4.092444444444444329, -0.3119999999999999996 ) ) ;
#13165 = CARTESIAN_POINT ( 'NONE',  ( 5.253288188650943643E-17, 5.197747365142496356, 0.2859756893339090444 ) ) ;
#13166 = CARTESIAN_POINT ( 'NONE',  ( -0.2206173157302027676, 4.557722222222221120, 0.2206173157302028787 ) ) ;
#13167 = VECTOR ( 'NONE', #5030, 39.37007874015748143 ) ;
#13168 = CARTESIAN_POINT ( 'NONE',  ( 0.2819296736111110979, 3.828555555631420582, -0.1167790944451423396 ) ) ;
#13169 = CARTESIAN_POINT ( 'NONE',  ( -0.2206173157302027676, 4.224388888888888083, 0.2206173157302028787 ) ) ;
#13170 = CARTESIAN_POINT ( 'NONE',  ( 0.1874014852520086982, 4.021786705011994201, 0.2494495279341875649 ) ) ;
#13171 = FACE_OUTER_BOUND ( 'NONE', #15551, .T. ) ;
#13172 = CARTESIAN_POINT ( 'NONE',  ( 0.1892591419382505802, 4.593624869007159717, -0.2515320889428918072 ) ) ;
#13173 = ORIENTED_EDGE ( 'NONE', *, *, #124, .T. ) ;
#13174 = PRODUCT_DEFINITION ( 'UNKNOWN', '', #4493, #9986 ) ;
#13175 = CARTESIAN_POINT ( 'NONE',  ( -0.3125000000000000000, 0.000000000000000000, 1.326383476483184332 ) ) ;
#13176 = CARTESIAN_POINT ( 'NONE',  ( 0.1641670432182899542, 4.150053599719361053, -0.2682616677331741695 ) ) ;
#13177 = CARTESIAN_POINT ( 'NONE',  ( 0.2230971623002954429, 0.2230971623002953319, -0.1217361111111106980 ) ) ;
#13178 = AXIS2_PLACEMENT_3D ( 'NONE', #16836, #14653, #9273 ) ;
#13179 = DIRECTION ( 'NONE',  ( -0.8660254037844434816, -2.725147086360870403E-18, 0.4999999999999913403 ) ) ;
#13180 = CARTESIAN_POINT ( 'NONE',  ( 0.1518731547439844121, 5.135423329234196643, 0.2660310188109448193 ) ) ;
#13181 = ORIENTED_EDGE ( 'NONE', *, *, #3978, .T. ) ;
#13182 = CARTESIAN_POINT ( 'NONE',  ( -0.1116596296178199582, 0.3187499999024575592, -0.3436530038418508792 ) ) ;
#13183 = CARTESIAN_POINT ( 'NONE',  ( 0.2819296736111110424, 0.3166666665908000056, -0.1167790944451423119 ) ) ;
#13184 = CARTESIAN_POINT ( 'NONE',  ( 0.3125000000000004996, 0.1294417382415917750, 0.1543055555555580549 ) ) ;
#13185 = CARTESIAN_POINT ( 'NONE',  ( 0.2825004670929462391, 0.6102487556800120228, -1.091766657629984483 ) ) ;
#13186 = DIRECTION ( 'NONE',  ( 0.000000000000000000, 0.000000000000000000, -1.000000000000000000 ) ) ;
#13187 = CARTESIAN_POINT ( 'NONE',  ( 0.1954553509668047195, 0.1954553509668046085, 0.01888888888889020401 ) ) ;
#13188 = CARTESIAN_POINT ( 'NONE',  ( -0.08047735155459137535, 5.094302086351763847, -0.3013681618867503076 ) ) ;
#13189 = CARTESIAN_POINT ( 'NONE',  ( -0.1292346314604044810, 4.727861111111109516, 0.3120000000000012208 ) ) ;
#13190 = CARTESIAN_POINT ( 'NONE',  ( -0.1292346314604056190, 0.1465277777777774515, -0.3119999999999999996 ) ) ;
#13191 = CARTESIAN_POINT ( 'NONE',  ( 0.2206173157302027954, 5.196611111111110404, -0.2206173157302028232 ) ) ;
#13192 = EDGE_CURVE ( 'NONE', #9761, #6190, #12094, .T. ) ;
#13193 = CARTESIAN_POINT ( 'NONE',  ( 0.1993543840281267465, 4.165361111186976828, 0.1993543840281266633 ) ) ;
#13194 = DIRECTION ( 'NONE',  ( -0.000000000000000000, -1.000000000000000000, -0.000000000000000000 ) ) ;
#13195 = DIRECTION ( 'NONE',  ( 0.000000000000000000, 0.000000000000000000, -1.000000000000000000 ) ) ;
#13196 = VERTEX_POINT ( 'NONE', #1882 ) ;
#13197 = AXIS2_PLACEMENT_3D ( 'NONE', #17125, #4307, #11763 ) ;
#13198 = LINE ( 'NONE', #11354, #22569 ) ;
#13199 = CARTESIAN_POINT ( 'NONE',  ( 0.2819296736111110979, 5.047305555631421470, -3.452642723725051716E-17 ) ) ;
#13200 = EDGE_CURVE ( 'NONE', #8250, #11335, #13126, .T. ) ;
#13201 = CARTESIAN_POINT ( 'NONE',  ( -0.3125000000000000000, 1.913510623667739771E-17, 0.01194444444444589179 ) ) ;
#13202 = CARTESIAN_POINT ( 'NONE',  ( 1.573500000000000343, -3.414809992080329023E-17, -1.412500000000000089 ) ) ;
#13203 = CARTESIAN_POINT ( 'NONE',  ( -0.09435543239135868454, -0.003009961218012348859, 2.763260016782451700 ) ) ;
#13204 = CARTESIAN_POINT ( 'NONE',  ( 0.1167790944451424506, 4.648000000075865223, 0.2819296736111110424 ) ) ;
#13205 = APPROVAL_ROLE ( '' ) ;
#13206 = CARTESIAN_POINT ( 'NONE',  ( -0.4620259694561341668, 0.2880908832651660756, 0.04413116910602139092 ) ) ;
#13207 =( BOUNDED_CURVE ( )  B_SPLINE_CURVE ( 2, ( #8658, #21826, #9028 ),
 .UNSPECIFIED., .F., .T. ) 
 B_SPLINE_CURVE_WITH_KNOTS ( ( 3, 3 ),
 ( 0.000000000000000000, 0.005292957132939934278 ),
 .UNSPECIFIED. ) 
 CURVE ( )  GEOMETRIC_REPRESENTATION_ITEM ( )  RATIONAL_B_SPLINE_CURVE ( ( 1.000000000000000000, 0.4999999999999998335, 1.000000000000000000 ) ) 
 REPRESENTATION_ITEM ( '' )  );
#13208 = CARTESIAN_POINT ( 'NONE',  ( 0.1144950937579609085, -0.2764156081756484751, 0.05708333333333493603 ) ) ;
#13209 =( BOUNDED_CURVE ( )  B_SPLINE_CURVE ( 2, ( #20287, #4263, #10904, #15486, #18334, #14689, #22107, #18450, #1746 ),
 .UNSPECIFIED., .F., .F. ) 
 B_SPLINE_CURVE_WITH_KNOTS ( ( 3, 2, 2, 2, 3 ),
 ( 0.6875000000000000000, 0.6979166666666666297, 0.7083333333333333703, 0.7187500000000000000, 0.7291666666666666297 ),
 .UNSPECIFIED. ) 
 CURVE ( )  GEOMETRIC_REPRESENTATION_ITEM ( )  RATIONAL_B_SPLINE_CURVE ( ( 1.000000000000000000, 0.9238795325112867385, 1.000000000000000000, 0.9238795325112867385, 1.000000000000000000, 0.9238795325112867385, 1.000000000000000000, 0.9238795325112867385, 1.000000000000000000 ) ) 
 REPRESENTATION_ITEM ( '' )  );
#13210 = CARTESIAN_POINT ( 'NONE',  ( -0.1993543840281266633, 0.4590277777019111105, -0.1993543840281266910 ) ) ;
#13212 = ORIENTED_EDGE ( 'NONE', *, *, #2764, .F. ) ;
#13211 = CIRCLE ( 'NONE', #19040, 0.01875000000000000625 ) ;
#13213 = ORIENTED_EDGE ( 'NONE', *, *, #12930, .F. ) ;
#13214 = CARTESIAN_POINT ( 'NONE',  ( 1.726321361862525858E-17, 0.2854166665908000056, -0.2819296736111110979 ) ) ;
#13215 = DIRECTION ( 'NONE',  ( -1.000000000000000000, 0.000000000000000000, 0.000000000000000000 ) ) ;
#13216 = FACE_OUTER_BOUND ( 'NONE', #13050, .T. ) ;
#13217 = CARTESIAN_POINT ( 'NONE',  ( 0.3999999999999999667, 0.1178571428571428270, -0.1299678784931625475 ) ) ;
#13218 = CARTESIAN_POINT ( 'NONE',  ( -0.3155070326520293400, 0.1306872919485614903, -0.05229166666666613256 ) ) ;
#13219 = CARTESIAN_POINT ( 'NONE',  ( -0.1966284714786305232, -0.4277423764267367923, 0.07944889038203660492 ) ) ;
#13220 = CARTESIAN_POINT ( 'NONE',  ( 0.1993543840281266910, 0.2645833332574666907, -0.1993543840281266910 ) ) ;
#13221 = CARTESIAN_POINT ( 'NONE',  ( 0.2819296736111110424, 0.08749999992413336203, 0.1167790944451424923 ) ) ;
#13222 = EDGE_CURVE ( 'NONE', #2181, #11779, #16878, .T. ) ;
#13223 = CARTESIAN_POINT ( 'NONE',  ( 0.2819296736111110979, 4.394527777853643791, -3.452642723725051716E-17 ) ) ;
#13224 = CARTESIAN_POINT ( 'NONE',  ( 0.2472135954999579721, 0.04464285694777236219, -0.3402603233408159622 ) ) ;
#13225 = CARTESIAN_POINT ( 'NONE',  ( 0.1167790944451424368, 4.939666666742532186, 0.2819296736111110424 ) ) ;
#13226 = CARTESIAN_POINT ( 'NONE',  ( -0.2819296736111110979, 4.352861111186976828, 0.000000000000000000 ) ) ;
#13227 = DIRECTION ( 'NONE',  ( -0.8660254037844433705, 0.000000000000000000, 0.4999999999999917843 ) ) ;
#13228 = CARTESIAN_POINT ( 'NONE',  ( 0.1615724546837533915, 3.909701830292296787, 0.2693711506783711407 ) ) ;
#13229 = CARTESIAN_POINT ( 'NONE',  ( -0.2206173157302027676, 4.175777777929510215, 0.2206173157302028787 ) ) ;
#13230 = ADVANCED_FACE ( 'NONE', ( #5780 ), #20775, .T. ) ;
#13231 = CARTESIAN_POINT ( 'NONE',  ( -0.3236067977499790249, 0.2910714283763437549, 0.2351141009169892271 ) ) ;
#13232 = VECTOR ( 'NONE', #11444, 39.37007874015748854 ) ;
#13233 = CARTESIAN_POINT ( 'NONE',  ( 0.2460300421372865198, -0.1745426587113542150, -0.09035713772767853258 ) ) ;
#13234 = ORIENTED_EDGE ( 'NONE', *, *, #1111, .T. ) ;
#13235 = PERSON_AND_ORGANIZATION ( #15518, #2538 ) ;
#13236 = EDGE_CURVE ( 'NONE', #21079, #20226, #11279, .T. ) ;
#13237 = CARTESIAN_POINT ( 'NONE',  ( 2.936000000000001720, 2.740000000000000213, -2.516000000000000014 ) ) ;
#13238 = LINE ( 'NONE', #11392, #13582 ) ;
#13239 = VERTEX_POINT ( 'NONE', #169 ) ;
#13240 = CARTESIAN_POINT ( 'NONE',  ( -0.1292346314604056190, 0.5284722220704892726, -0.3119999999999999996 ) ) ;
#13241 = ORIENTED_EDGE ( 'NONE', *, *, #7969, .F. ) ;
#13242 = CARTESIAN_POINT ( 'NONE',  ( -0.3125000000000000000, 1.913510623667739771E-17, 0.1786111111111139127 ) ) ;
#13243 = CARTESIAN_POINT ( 'NONE',  ( 0.05904265200914168149, 4.764370636974210704, -0.3065873589144272882 ) ) ;
#13244 = CARTESIAN_POINT ( 'NONE',  ( -0.2923287055106771337, -0.03482142866897096345, 0.2123892367102619971 ) ) ;
#13245 = LINE ( 'NONE', #3589, #19807 ) ;
#13246 = ORIENTED_EDGE ( 'NONE', *, *, #13947, .F. ) ;
#13247 = CARTESIAN_POINT ( 'NONE',  ( 0.3613381517857143232, 0.1580357141881718608, -0.1174058825155740587 ) ) ;
#13248 = AXIS2_PLACEMENT_3D ( 'NONE', #10485, #21565, #11969 ) ;
#13249 = ORIENTED_EDGE ( 'NONE', *, *, #16183, .F. ) ;
#13250 = CYLINDRICAL_SURFACE ( 'NONE', #1026, 0.2500000000000000000 ) ;
#13251 = CARTESIAN_POINT ( 'NONE',  ( -0.2983457502834188646, 4.666223328268666037, -0.09148694476314270241 ) ) ;
#13252 = CARTESIAN_POINT ( 'NONE',  ( 0.1167790944451422702, 3.891055555631421914, -0.2819296736111110424 ) ) ;
#13253 = CARTESIAN_POINT ( 'NONE',  ( -0.4622078388679875527, -0.2744100571732869254, 0.3892820121258429023 ) ) ;
#13254 = FACE_OUTER_BOUND ( 'NONE', #17750, .T. ) ;
#13255 = CARTESIAN_POINT ( 'NONE',  ( 0.2206173157302028787, 3.793833333333332725, 0.2206173157302027954 ) ) ;
#13256 = ADVANCED_FACE ( 'NONE', ( #1642 ), #7729, .F. ) ;
#13257 = CARTESIAN_POINT ( 'NONE',  ( 0.3119999999999999996, 4.804250000151731648, 0.1292346314604056190 ) ) ;
#13258 = EDGE_CURVE ( 'NONE', #17766, #13298, #1514, .T. ) ;
#13259 = CARTESIAN_POINT ( 'NONE',  ( 0.1167790944451424506, 5.161888888964753619, 0.2819296736111110424 ) ) ;
#13260 = CARTESIAN_POINT ( 'NONE',  ( 0.2819296736111110424, 4.217444444520310753, -0.1167790944451423396 ) ) ;
#13261 = DIRECTION ( 'NONE',  ( 0.000000000000000000, 0.000000000000000000, -1.000000000000000000 ) ) ;
#13262 = CARTESIAN_POINT ( 'NONE',  ( 0.3613381517857143232, 0.06160714275960043479, 0.1174058825155741975 ) ) ;
#13263 = VERTEX_POINT ( 'NONE', #22358 ) ;
#13264 = TOROIDAL_SURFACE ( 'NONE', #2728, 0.2510000000000000009, 0.001000000000000038835 ) ;
#13265 = ORIENTED_EDGE ( 'NONE', *, *, #14761, .T. ) ;
#13266 = PERSON_AND_ORGANIZATION_ROLE ( 'classification_officer' ) ;
#13267 = FACE_OUTER_BOUND ( 'NONE', #12415, .T. ) ;
#13268 = CARTESIAN_POINT ( 'NONE',  ( 0.1167790944451424368, 5.036888888964754507, 0.2819296736111110424 ) ) ;
#13269 = CARTESIAN_POINT ( 'NONE',  ( -0.2819296736111110979, 3.922305555631421914, 0.000000000000000000 ) ) ;
#13270 = CARTESIAN_POINT ( 'NONE',  ( 0.2152754385359916256, 4.411674947035939987, 0.2271887073179320593 ) ) ;
#13271 = ORIENTED_EDGE ( 'NONE', *, *, #7063, .F. ) ;
#13272 = CARTESIAN_POINT ( 'NONE',  ( -0.1954553509668046918, -0.1954553509668046640, 0.2619444444444477549 ) ) ;
#13273 = CARTESIAN_POINT ( 'NONE',  ( -0.1167790944451422702, 0.5111111110352445364, -0.2819296736111110979 ) ) ;
#13274 = CARTESIAN_POINT ( 'NONE',  ( -0.1144950937579609779, 0.2764156081756484196, 0.3626388888888929518 ) ) ;
#13275 = CARTESIAN_POINT ( 'NONE',  ( 0.2819296736111110424, 5.009111111186976828, -0.1167790944451423396 ) ) ;
#13276 = CARTESIAN_POINT ( 'NONE',  ( -0.004187250022457828999, -0.5383673285787258234, 0.04698409998688798245 ) ) ;
#13277 = CARTESIAN_POINT ( 'NONE',  ( 0.2819296736111110424, 4.939666666742532186, -0.1167790944451423396 ) ) ;
#13278 = CARTESIAN_POINT ( 'NONE',  ( 1.750236327630675537E-16, 0.08749999980491518503, 0.3999999999999999667 ) ) ;
#13279 = VECTOR ( 'NONE', #4757, 39.37007874015748143 ) ;
#13280 = LINE ( 'NONE', #10454, #1181 ) ;
#13281 = CARTESIAN_POINT ( 'NONE',  ( -0.001863919267159286786, 1.041821957232212270, -2.908070964936878333 ) ) ;
#13282 = CARTESIAN_POINT ( 'NONE',  ( -0.1060554323913586589, -0.003009961218012348859, 2.783525011231007706 ) ) ;
#13283 = CARTESIAN_POINT ( 'NONE',  ( 0.2206173157302027954, 4.474388888888888083, -0.2206173157302028232 ) ) ;
#13284 = CARTESIAN_POINT ( 'NONE',  ( 0.1900105704308386045, 5.206640035683666845, 0.2082794372640154323 ) ) ;
#13285 = CIRCLE ( 'NONE', #14844, 0.7650000000000000133 ) ;
#13286 = CARTESIAN_POINT ( 'NONE',  ( 0.1167790944451422702, 3.835500000075866112, -0.2819296736111110979 ) ) ;
#13287 = DIRECTION ( 'NONE',  ( -0.000000000000000000, -1.000000000000000000, -0.000000000000000000 ) ) ;
#13288 = CARTESIAN_POINT ( 'NONE',  ( 0.000000000000000000, 5.384999999999999787, 0.000000000000000000 ) ) ;
#13289 = CARTESIAN_POINT ( 'NONE',  ( 0.000000000000000000, 5.384999999999999787, 0.000000000000000000 ) ) ;
#13290 = DIRECTION ( 'NONE',  ( -0.000000000000000000, -1.000000000000000000, -0.000000000000000000 ) ) ;
#13291 = CARTESIAN_POINT ( 'NONE',  ( -0.1462652582317430505, 4.103741065394783227, -0.2781719402188991275 ) ) ;
#13292 = CARTESIAN_POINT ( 'NONE',  ( 0.09033206243994013063, 4.629811855264434506, 0.3017044624047845458 ) ) ;
#13293 = EDGE_CURVE ( 'NONE', #16468, #23807, #18709, .T. ) ;
#13294 = CARTESIAN_POINT ( 'NONE',  ( 0.2230971623002953874, -0.2230971623002954429, -0.08006944444444370756 ) ) ;
#13295 = CIRCLE ( 'NONE', #10948, 0.2495000000000007212 ) ;
#13296 = CARTESIAN_POINT ( 'NONE',  ( 0.2496269975438151767, 4.313450179719811928, -0.1915744269021862900 ) ) ;
#13297 = CARTESIAN_POINT ( 'NONE',  ( 0.1769619725182808578, 5.155811688406484627, -0.2434508416669157460 ) ) ;
#13298 = VERTEX_POINT ( 'NONE', #13242 ) ;
#13299 = CARTESIAN_POINT ( 'NONE',  ( -0.2923287055106771337, 0.1973214284738861179, 0.2123892367102619971 ) ) ;
#13300 = CARTESIAN_POINT ( 'NONE',  ( 0.2819296736111110424, 0.5319444443685777957, 0.1167790944451424923 ) ) ;
#13301 = CARTESIAN_POINT ( 'NONE',  ( -7.892860322346445127E-13, 5.206640035683665957, 0.2819296736111106538 ) ) ;
#13302 = CARTESIAN_POINT ( 'NONE',  ( 0.3068681509333300861, 0.5432192738334535864, -1.103814563215323785 ) ) ;
#13303 = CARTESIAN_POINT ( 'NONE',  ( 0.000000000000000000, 0.7650000000000000133, 0.000000000000000000 ) ) ;
#13304 = CARTESIAN_POINT ( 'NONE',  ( -0.2764156081756484196, -0.1144950937579609362, 0.09875000000000193345 ) ) ;
#13305 = CARTESIAN_POINT ( 'NONE',  ( 0.3247595264191642794, 2.291712385858714729, -0.9871846966950100777 ) ) ;
#13306 = DIRECTION ( 'NONE',  ( 1.000000000000000000, 0.000000000000000000, 0.000000000000000000 ) ) ;
#13307 = CARTESIAN_POINT ( 'NONE',  ( -0.1292346314604058410, 0.2229166666666664021, 0.3119999999999998885 ) ) ;
#13308 = CARTESIAN_POINT ( 'NONE',  ( 0.1292346314604058410, 5.123694444444443441, 0.3119999999999998885 ) ) ;
#13309 = CARTESIAN_POINT ( 'NONE',  ( 0.2819296736111110979, 4.168833333409199149, 0.1167790944451422425 ) ) ;
#13310 = FACE_OUTER_BOUND ( 'NONE', #8913, .T. ) ;
#13311 = AXIS2_PLACEMENT_3D ( 'NONE', #104, #14879, #5593 ) ;
#13312 = EDGE_LOOP ( 'NONE', ( #1753, #9212, #4362, #11071 ) ) ;
#13313 = CARTESIAN_POINT ( 'NONE',  ( 0.1236067977499789861, 0.3339285712334865708, -0.3804226065180614236 ) ) ;
#13314 = CARTESIAN_POINT ( 'NONE',  ( 0.1167790944451422702, 4.891055555631421470, -0.2819296736111110424 ) ) ;
#13315 = CARTESIAN_POINT ( 'NONE',  ( 0.2346572839409867828, 4.190181929725985022, 0.2066278427949707619 ) ) ;
#13316 = CARTESIAN_POINT ( 'NONE',  ( 1.573500000000000565, 2.740000000000000213, -1.412500000000000311 ) ) ;
#13317 = DIRECTION ( 'NONE',  ( -0.4999999999999912292, 0.000000000000000000, 0.8660254037844437036 ) ) ;
#13318 = CARTESIAN_POINT ( 'NONE',  ( -0.2819296736111110979, 4.686194444520309865, 0.000000000000000000 ) ) ;
#13319 = CARTESIAN_POINT ( 'NONE',  ( 8.643737792453333225E-17, -0.5196152422706635798, 0.3779506566538943235 ) ) ;
#13320 = CARTESIAN_POINT ( 'NONE',  ( -0.2764156081756484196, 1.692557448933383907E-17, 0.03972222222222369925 ) ) ;
#13321 = CARTESIAN_POINT ( 'NONE',  ( 0.2819296736111110979, 0.6048611110352445364, 0.000000000000000000 ) ) ;
#13322 = ORIENTED_EDGE ( 'NONE', *, *, #10070, .F. ) ;
#13323 = CARTESIAN_POINT ( 'NONE',  ( 0.2819296736111110979, 0.4937499999241333204, 0.000000000000000000 ) ) ;
#13324 = CARTESIAN_POINT ( 'NONE',  ( 0.4116666666666667918, 2.681666666666666643, -2.557666666666666533 ) ) ;
#13325 = CYLINDRICAL_SURFACE ( 'NONE', #4304, 0.3119999999999999996 ) ;
#13326 = CARTESIAN_POINT ( 'NONE',  ( -0.1236067977499789583, 0.2071428571428570731, -0.3804226065180614791 ) ) ;
#13327 = CARTESIAN_POINT ( 'NONE',  ( 0.3155070326520292290, -0.1306872919485616569, 0.1977083333333359005 ) ) ;
#13328 = EDGE_CURVE ( 'NONE', #7496, #19658, #11038, .T. ) ;
#13329 = CARTESIAN_POINT ( 'NONE',  ( -0.1650495903302308942, -0.4585922144775718690, 0.07156651416104609087 ) ) ;
#13330 = PLANE ( 'NONE',  #14824 ) ;
#13331 = CARTESIAN_POINT ( 'NONE',  ( 0.2819296736111110979, 0.2576388888130222155, 0.000000000000000000 ) ) ;
#13332 = CARTESIAN_POINT ( 'NONE',  ( -0.1167790944451424368, 0.1847222221463556413, 0.2819296736111110424 ) ) ;
#13333 = ORIENTED_EDGE ( 'NONE', *, *, #7522, .F. ) ;
#13334 = CARTESIAN_POINT ( 'NONE',  ( 0.1167790944451424368, 4.328555555631420582, 0.2819296736111110424 ) ) ;
#13335 = CARTESIAN_POINT ( 'NONE',  ( 0.2472135954999579721, 0.1874999998049151628, -0.3402603233408159622 ) ) ;
#13336 = CARTESIAN_POINT ( 'NONE',  ( -0.2819296736111110979, 4.977861111186976828, 0.000000000000000000 ) ) ;
#13337 = CARTESIAN_POINT ( 'NONE',  ( 5.178964085587577574E-17, 4.533416666742532186, 0.2819296736111110979 ) ) ;
#13338 = CARTESIAN_POINT ( 'NONE',  ( 1.573500000000000343, 2.683750000000000746, -1.412500000000000089 ) ) ;
#13339 = LINE ( 'NONE', #6242, #14013 ) ;
#13340 = CARTESIAN_POINT ( 'NONE',  ( -0.1292346314604056745, 4.158416666818398610, -0.3119999999999999996 ) ) ;
#13341 = CARTESIAN_POINT ( 'NONE',  ( 1.840071746775174377, 2.291712385858714285, -2.386288568296996981 ) ) ;
#13342 = ORIENTED_EDGE ( 'NONE', *, *, #22582, .F. ) ;
#13343 = EDGE_CURVE ( 'NONE', #15982, #22290, #7610, .T. ) ;
#13344 = EDGE_CURVE ( 'NONE', #1661, #13614, #3586, .T. ) ;
#13345 = APPROVAL_DATE_TIME ( #18947, #22804 ) ;
#13346 = ORIENTED_EDGE ( 'NONE', *, *, #10509, .T. ) ;
#13347 = AXIS2_PLACEMENT_3D ( 'NONE', #3625, #1920, #20219 ) ;
#13348 = CARTESIAN_POINT ( 'NONE',  ( 0.1458082941847509140, 0.2460910087212031805, 0.3975519585608662254 ) ) ;
#13349 = PLANE ( 'NONE',  #17721 ) ;
#13350 = CARTESIAN_POINT ( 'NONE',  ( -0.5116234456863258950, 4.730490217694243604, -2.640781157734872320 ) ) ;
#13351 = ORIENTED_EDGE ( 'NONE', *, *, #8759, .T. ) ;
#13352 = CARTESIAN_POINT ( 'NONE',  ( -0.3119999999999999996, 0.5979166665149336923, 0.1292346314604056190 ) ) ;
#13353 = ORIENTED_EDGE ( 'NONE', *, *, #24008, .T. ) ;
#13354 = DIRECTION ( 'NONE',  ( 0.000000000000000000, 0.7071067811865474617, 0.7071067811865474617 ) ) ;
#13355 = CARTESIAN_POINT ( 'NONE',  ( 0.000000000000000000, 5.384999999999999787, -0.3119999999999999996 ) ) ;
#13356 = CARTESIAN_POINT ( 'NONE',  ( 0.02086467461746857599, 4.765462960542953041, -0.3114012365584180042 ) ) ;
#13357 = CARTESIAN_POINT ( 'NONE',  ( -0.1116596296178200276, 0.1151785713310290032, 0.3436530038418508792 ) ) ;
#13358 = DIRECTION ( 'NONE',  ( 0.000000000000000000, 1.000000000000000000, 0.000000000000000000 ) ) ;
#13359 = EDGE_CURVE ( 'NONE', #8579, #7946, #11396, .T. ) ;
#13360 = ORIENTED_EDGE ( 'NONE', *, *, #2235, .F. ) ;
#13361 = CARTESIAN_POINT ( 'NONE',  ( -0.2923287055106771337, 0.3258928570453146767, -0.2123892367102620804 ) ) ;
#13362 = FACE_OUTER_BOUND ( 'NONE', #5282, .T. ) ;
#13363 = CARTESIAN_POINT ( 'NONE',  ( -0.1954553509668046918, -0.1954553509668046640, 0.4286111111111157168 ) ) ;
#13364 = CARTESIAN_POINT ( 'NONE',  ( -0.1993543840281266355, 3.915361111186976384, 0.1993543840281267465 ) ) ;
#13365 = CARTESIAN_POINT ( 'NONE',  ( 0.2206290632986846467, 5.036984000381125703, -0.2218005928150467154 ) ) ;
#13366 = CARTESIAN_POINT ( 'NONE',  ( -0.1292346314604093660, 4.818138888888888083, -0.3119999999999962803 ) ) ;
#13367 = CARTESIAN_POINT ( 'NONE',  ( 0.1988757138996042617, 3.752970977545328601, -0.2404006040361021113 ) ) ;
#13368 = CARTESIAN_POINT ( 'NONE',  ( 0.3119999999999999996, 4.696611111262843252, -3.820898013339742174E-17 ) ) ;
#13369 = CIRCLE ( 'NONE', #19577, 0.2500000000000000555 ) ;
#13370 = CARTESIAN_POINT ( 'NONE',  ( -1.726321361862525858E-17, 4.908416666742532186, -0.2819296736111110979 ) ) ;
#13371 = ORIENTED_EDGE ( 'NONE', *, *, #12493, .T. ) ;
#13372 = EDGE_CURVE ( 'NONE', #6049, #21992, #11817, .T. ) ;
#13373 = CARTESIAN_POINT ( 'NONE',  ( 0.1167790944451422702, 4.279944444520310753, -0.2819296736111110424 ) ) ;
#13374 = ORIENTED_EDGE ( 'NONE', *, *, #15539, .T. ) ;
#13375 = CARTESIAN_POINT ( 'NONE',  ( -0.2923287055106771337, 0.09374999990245758141, -0.2123892367102620804 ) ) ;
#13376 = ORIENTED_EDGE ( 'NONE', *, *, #5088, .T. ) ;
#13377 = ORIENTED_EDGE ( 'NONE', *, *, #11870, .T. ) ;
#13378 = SHAPE_DEFINITION_REPRESENTATION ( #8550, #11202 ) ;
#13379 = CARTESIAN_POINT ( 'NONE',  ( -0.1306872919485614903, 0.3155070326520293400, 0.4442361111111159389 ) ) ;
#13380 = DIRECTION ( 'NONE',  ( 0.000000000000000000, 0.000000000000000000, 1.000000000000000000 ) ) ;
#13381 = CARTESIAN_POINT ( 'NONE',  ( -0.1167790944451423535, 3.932722222298087988, 0.2819296736111110979 ) ) ;
#13382 = CARTESIAN_POINT ( 'NONE',  ( 0.000000000000000000, 0.4199999999999998734, -0.2500000000000000555 ) ) ;
#13383 = CARTESIAN_POINT ( 'NONE',  ( -0.2764156081756484196, -0.1144950937579609362, 0.3209722222222259891 ) ) ;
#13384 = CARTESIAN_POINT ( 'NONE',  ( 0.09134320533036652257, -0.5015400784327699313, 0.06108448616840793377 ) ) ;
#13385 = ORIENTED_EDGE ( 'NONE', *, *, #8726, .T. ) ;
#13386 = CARTESIAN_POINT ( 'NONE',  ( -0.1954553509668046640, 0.1954553509668046918, 0.3036111111111147176 ) ) ;
#13387 = CARTESIAN_POINT ( 'NONE',  ( -0.2819296736111110979, 0.4069444443685778512, -0.1167790944451423396 ) ) ;
#13388 = CARTESIAN_POINT ( 'NONE',  ( -0.2764156081756484196, 0.1144950937579609918, -0.1373611111111110172 ) ) ;
#13389 = ORIENTED_EDGE ( 'NONE', *, *, #10580, .F. ) ;
#13390 = CARTESIAN_POINT ( 'NONE',  ( 0.1167790944451422702, 5.016055555631420582, -0.2819296736111110424 ) ) ;
#13391 = CARTESIAN_POINT ( 'NONE',  ( 0.2496181645126293036, 4.468611226231085531, 0.1915855071014845590 ) ) ;
#13392 = CARTESIAN_POINT ( 'NONE',  ( -0.2819296736111110424, 4.627166666742532186, -0.1167790944451423119 ) ) ;
#13393 = CARTESIAN_POINT ( 'NONE',  ( -0.1166234456863257940, 4.111524471938507119, -2.802594437230254254 ) ) ;
#13394 = CARTESIAN_POINT ( 'NONE',  ( 0.2099978738425454516, 4.855935259588629371, 0.2307503733689650338 ) ) ;
#13395 = CARTESIAN_POINT ( 'NONE',  ( 0.000000000000000000, 2.740000000000000213, -2.936000000000001720 ) ) ;
#13396 = CARTESIAN_POINT ( 'NONE',  ( 0.4679241437345806887, 0.2662683654317170578, 0.05892738626661209178 ) ) ;
#13397 = CARTESIAN_POINT ( 'NONE',  ( -1.910449006669871087E-17, 4.425777777777777366, -0.3119999999999999996 ) ) ;
#13398 = CARTESIAN_POINT ( 'NONE',  ( 5.178964085587577574E-17, 3.811194444520309865, 0.2819296736111110979 ) ) ;
#13399 = CARTESIAN_POINT ( 'NONE',  ( 0.3119999999999998885, 0.3409722220704892726, 0.1292346314604058410 ) ) ;
#13400 = FACE_OUTER_BOUND ( 'NONE', #20874, .T. ) ;
#13401 = ORIENTED_EDGE ( 'NONE', *, *, #8496, .F. ) ;
#13402 = CARTESIAN_POINT ( 'NONE',  ( 0.3109988355630948775, 4.584817533366577713, 0.02498716424996858324 ) ) ;
#13403 = ORIENTED_EDGE ( 'NONE', *, *, #5906, .T. ) ;
#13404 = CIRCLE ( 'NONE', #4809, 0.001000000000000037101 ) ;
#13405 = CARTESIAN_POINT ( 'NONE',  ( -0.2209708691207961373, -0.2209708691207961095, 0.07444444444444638098 ) ) ;
#13406 = CARTESIAN_POINT ( 'NONE',  ( 0.1954553509668047195, 0.1954553509668046085, 0.4008333333333377047 ) ) ;
#13407 = EDGE_CURVE ( 'NONE', #16373, #2537, #21261, .T. ) ;
#13408 = CARTESIAN_POINT ( 'NONE',  ( -0.3038794427342524362, 3.944299538033225527, -0.08166546517153733253 ) ) ;
#13409 = EDGE_CURVE ( 'NONE', #20523, #22475, #437, .T. ) ;
#13410 = ORIENTED_EDGE ( 'NONE', *, *, #10342, .T. ) ;
#13411 = CARTESIAN_POINT ( 'NONE',  ( -0.1116596296178199582, 0.08660714275960045005, -0.3436530038418508792 ) ) ;
#13412 = CARTESIAN_POINT ( 'NONE',  ( 1.726321361862525858E-17, 0.4937499999241333759, -0.2819296736111110979 ) ) ;
#13413 = LINE ( 'NONE', #17539, #810 ) ;
#13414 = CARTESIAN_POINT ( 'NONE',  ( 9.184850993605150903E-17, 2.735000000000000320, -0.7500000000000001110 ) ) ;
#13415 = CARTESIAN_POINT ( 'NONE',  ( 0.6288319206375506676, 7.738357572422988565E-17, 0.004799741732707325965 ) ) ;
#13416 = CARTESIAN_POINT ( 'NONE',  ( 0.1144950937579611444, 0.2764156081756483641, 0.1890277777777804036 ) ) ;
#13417 = AXIS2_PLACEMENT_3D ( 'NONE', #15098, #7528, #3987 ) ;
#13418 = VERTEX_POINT ( 'NONE', #18953 ) ;
#13419 = CARTESIAN_POINT ( 'NONE',  ( -0.04423000916681948252, 4.625947756500051078, 0.3119999933242569301 ) ) ;
#13420 = LINE ( 'NONE', #20841, #14433 ) ;
#13421 = CARTESIAN_POINT ( 'NONE',  ( 0.000000000000000000, 0.3125000000000000000, 0.3313888888888928408 ) ) ;
#13422 = CARTESIAN_POINT ( 'NONE',  ( 0.1292346314604056745, 0.3062499999999996336, -0.3119999999999999996 ) ) ;
#13423 = CARTESIAN_POINT ( 'NONE',  ( 0.5496543701456371167, 3.720840944996751887, 0.08881361666993904669 ) ) ;
#13424 =( REPRESENTATION_RELATIONSHIP ('NONE','NONE', #4490, #11202 ) REPRESENTATION_RELATIONSHIP_WITH_TRANSFORMATION ( #16960 )SHAPE_REPRESENTATION_RELATIONSHIP( ) );
#13425 = CARTESIAN_POINT ( 'NONE',  ( 0.2819296736111110979, 4.227861111186976828, -3.452642723725051716E-17 ) ) ;
#13426 = CARTESIAN_POINT ( 'NONE',  ( -0.04081697132525561461, 4.348175715971974498, 0.3120000054304696846 ) ) ;
#13427 = FACE_BOUND ( 'NONE', #1273, .T. ) ;
#13428 = FACE_OUTER_BOUND ( 'NONE', #1664, .T. ) ;
#13429 = ORIENTED_EDGE ( 'NONE', *, *, #9494, .T. ) ;
#13430 = ORIENTED_EDGE ( 'NONE', *, *, #19549, .F. ) ;
#13431 = CARTESIAN_POINT ( 'NONE',  ( 9.101228903679513089E-16, 0.3017857140906293756, 0.4000000000000000222 ) ) ;
#13432 = CARTESIAN_POINT ( 'NONE',  ( 0.1993543840281267465, 4.818138888964754507, 0.1993543840281266633 ) ) ;
#13433 = CARTESIAN_POINT ( 'NONE',  ( 0.04811092099939980049, 0.5134890241753962137, 0.05816431335571147637 ) ) ;
#13434 = CARTESIAN_POINT ( 'NONE',  ( 0.000000000000000000, 0.02999999999999995379, 0.000000000000000000 ) ) ;
#13435 = VECTOR ( 'NONE', #16957, 39.37007874015748854 ) ;
#13436 = DIRECTION ( 'NONE',  ( 0.2467484359828400475, -6.334534208364528778E-17, 0.9690795681160667696 ) ) ;
#13437 = CARTESIAN_POINT ( 'NONE',  ( 0.1395004180248995140, 3.706493199255800786, -0.2813810779009488505 ) ) ;
#13438 = APPROVAL ( #5294, 'UNSPECIFIED' ) ;
#13439 = FACE_OUTER_BOUND ( 'NONE', #15329, .T. ) ;
#13440 = CARTESIAN_POINT ( 'NONE',  ( 5.178964085587577574E-17, 4.213972222298087544, 0.2819296736111110979 ) ) ;
#13441 = PERSON_AND_ORGANIZATION_ROLE ( 'classification_officer' ) ;
#13442 = CARTESIAN_POINT ( 'NONE',  ( -0.2023794242524271647, 4.050101341561973989, -0.2374638867795466346 ) ) ;
#13443 = CARTESIAN_POINT ( 'NONE',  ( 0.1144950937579611444, 0.2764156081756483641, 0.02236111111111246594 ) ) ;
#13444 = LOCAL_TIME ( 21, 9, 13.00000000000000000, #15848 ) ;
#13445 = LINE ( 'NONE', #20863, #10661 ) ;
#13446 = ORIENTED_EDGE ( 'NONE', *, *, #23865, .T. ) ;
#13447 = CARTESIAN_POINT ( 'NONE',  ( -0.2819296736111110979, 0.5215277777019111660, -3.452642723725051716E-17 ) ) ;
#13448 = DIRECTION ( 'NONE',  ( -0.000000000000000000, -1.000000000000000000, -0.000000000000000000 ) ) ;
#13449 = DIRECTION ( 'NONE',  ( 0.000000000000000000, 0.000000000000000000, -1.000000000000000000 ) ) ;
#13450 = CARTESIAN_POINT ( 'NONE',  ( -0.4000000000000000222, 0.2249999999999999500, 0.1299678784931624920 ) ) ;
#13451 = CARTESIAN_POINT ( 'NONE',  ( -0.1306872919485614903, 0.3155070326520293400, 0.2740972222222253785 ) ) ;
#13452 = CARTESIAN_POINT ( 'NONE',  ( -0.2022257292156467434, -0.4370114112024232611, 0.07440066028686581623 ) ) ;
#13453 = CARTESIAN_POINT ( 'NONE',  ( 0.1292346314604045920, 5.012583333333331836, 0.3120000000000012208 ) ) ;
#13454 = CARTESIAN_POINT ( 'NONE',  ( 0.1993543840281266355, 0.5284722221463555858, 0.1993543840281267465 ) ) ;
#13455 = B_SPLINE_CURVE_WITH_KNOTS ( 'NONE', 3,
 ( #2116, #22717, #20413, #9557, #18585, #9318, #16758, #14934, #22353, #5657, #13121, #11272, #18703, #2002, #9439, #163, #7605, #8894, #15972, #17924, #18040, #4745, #6700, #1219, #21702, #10382, #19991, #17683, #23151, #10731, #6949, #12450, #6462, #12099, #18162, #23631, #13916, #6824, #19869, #23270, #8528, #21574, #4868, #8647, #16095, #12216, #10494, #3161, #1096, #14265, #4985 ),
 .UNSPECIFIED., .F., .F.,
 ( 4, 2, 2, 2, 1, 1, 2, 2, 1, 2, 2, 2, 2, 1, 1, 2, 2, 2, 2, 2, 2, 2, 2, 2, 1, 1, 1, 1, 2, 4 ),
 ( 0.2471660779490366389, 0.2482799422568952308, 0.2488368744108245545, 0.2491153404877891886, 0.2492545735262715334, 0.2493241900455126780, 0.2493589983051332781, 0.2493764024349435504, 0.2493938065647538505, 0.2516215351804711453, 0.2538492637961884957, 0.2549631281040471431, 0.2560769924119057905, 0.2562162254503881353, 0.2562858419696293355, 0.2563206502292498801, 0.2563554584888704801, 0.2566339245658351698, 0.2571908567197644935, 0.2583047210276230854, 0.2605324496433403803, 0.2627601782590576751, 0.2638740425669163225, 0.2644309747208456463, 0.2647094407978103359, 0.2648486738362926252, 0.2649182903555338253, 0.2649530986151543699, 0.2649705027449646977, 0.2649879068747749700 ),
 .UNSPECIFIED. ) ;
#13456 = CARTESIAN_POINT ( 'NONE',  ( 0.1167790944451423257, 0.1569444443685778234, -0.2819296736111110424 ) ) ;
#13457 = CARTESIAN_POINT ( 'NONE',  ( -0.2819296736111110979, 4.255638888964754507, 0.000000000000000000 ) ) ;
#13459 = B_SPLINE_CURVE_WITH_KNOTS ( 'NONE', 3,
 ( #18628, #18385, #9113, #21799, #16563, #24105, #14866, #20459, #3756, #16202, #7885, #18750, #15217, #571, #9728, #16807, #22402, #9608 ),
 .UNSPECIFIED., .F., .F.,
 ( 4, 2, 2, 2, 2, 2, 2, 2, 4 ),
 ( 6.938893903907228378E-18, 0.001843124596548163753, 0.003686249193096320566, 0.005529373789644477163, 0.007372498386192625520, 0.009215622982740773877, 0.01105874757928892137, 0.01290187217583707233, 0.01474499677238521808 ),
 .UNSPECIFIED. ) ;
#13458 = CARTESIAN_POINT ( 'NONE',  ( -0.3236067977499789694, 0.2053571426620580676, -0.2351141009169893104 ) ) ;
#13460 = CARTESIAN_POINT ( 'NONE',  ( -0.1993543840281266910, 4.859805555631421470, -0.1993543840281266910 ) ) ;
#13461 = CARTESIAN_POINT ( 'NONE',  ( 0.1993543840281266633, 4.276472222298087544, -0.1993543840281266910 ) ) ;
#13462 = EDGE_CURVE ( 'NONE', #19562, #11776, #11642, .T. ) ;
#13463 = PLANE ( 'NONE',  #23065 ) ;
#13464 = CARTESIAN_POINT ( 'NONE',  ( -0.2209708691207961373, -0.2209708691207961095, 0.2341666666666694929 ) ) ;
#13465 = CARTESIAN_POINT ( 'NONE',  ( 0.2206173157302028787, 3.967444444596176734, 0.2206173157302027954 ) ) ;
#13466 = CARTESIAN_POINT ( 'NONE',  ( 0.2206173157302028232, 0.1361111111111107663, -0.2206173157302028232 ) ) ;
#13467 = EDGE_CURVE ( 'NONE', #6124, #7372, #15295, .T. ) ;
#13468 = CARTESIAN_POINT ( 'NONE',  ( 0.1898046044843661184, -0.2363956207629887840, -0.09186489914520645783 ) ) ;
#13469 = VERTEX_POINT ( 'NONE', #4190 ) ;
#13470 = CARTESIAN_POINT ( 'NONE',  ( 1.573500000000000343, -3.414809992080329023E-17, -0.9499999999999999556 ) ) ;
#13471 = PERSON_AND_ORGANIZATION ( #15518, #2538 ) ;
#13472 = EDGE_LOOP ( 'NONE', ( #18367, #15671, #21970 ) ) ;
#13473 = AXIS2_PLACEMENT_3D ( 'NONE', #9332, #14945, #20309 ) ;
#13474 = LINE ( 'NONE', #6374, #7044 ) ;
#13475 = LINE ( 'NONE', #2246, #22776 ) ;
#13476 = CARTESIAN_POINT ( 'NONE',  ( -0.3466234456863258040, 5.071846480923144718, -2.736043952151160141 ) ) ;
#13477 = VERTEX_POINT ( 'NONE', #19067 ) ;
#13478 = CARTESIAN_POINT ( 'NONE',  ( 0.1292346314604056745, 0.4659722220704892726, -0.3119999999999999996 ) ) ;
#13479 = ORIENTED_EDGE ( 'NONE', *, *, #4382, .F. ) ;
#13480 = CARTESIAN_POINT ( 'NONE',  ( -0.3236067977499789694, -1.707404996040164512E-17, -0.2351141009169893104 ) ) ;
#13481 = CARTESIAN_POINT ( 'NONE',  ( 0.4251436100156877895, 0.2958090996783798721, 0.4013701042764563076 ) ) ;
#13482 = LINE ( 'NONE', #11764, #21021 ) ;
#13483 = CARTESIAN_POINT ( 'NONE',  ( -0.3613381517857143232, 0.02589285704531474330, -0.1174058825155741004 ) ) ;
#13484 = CARTESIAN_POINT ( 'NONE',  ( 0.1712376643660483699, 5.185778304708162700, -0.2353596117731020232 ) ) ;
#13485 = ORIENTED_EDGE ( 'NONE', *, *, #19811, .F. ) ;
#13486 = CC_DESIGN_APPROVAL ( #5204, ( #582 ) ) ;
#13487 = CARTESIAN_POINT ( 'NONE',  ( -0.3613381517857143232, 0.2616071427596003973, -4.425116109941954795E-17 ) ) ;
#13488 = CARTESIAN_POINT ( 'NONE',  ( 0.000000000000000000, 3.738758431839877614E-19, -0.1016666666666665164 ) ) ;
#13489 = CARTESIAN_POINT ( 'NONE',  ( 0.1954553509668046640, -0.1954553509668047195, 0.4425000000000047229 ) ) ;
#13490 = CARTESIAN_POINT ( 'NONE',  ( 5.178964085587577574E-17, 3.977861111186976384, 0.2819296736111110979 ) ) ;
#13491 = CARTESIAN_POINT ( 'NONE',  ( -0.2142276530138171042, -0.4175814842298855023, 0.4181133580835095231 ) ) ;
#13492 = CARTESIAN_POINT ( 'NONE',  ( 0.09872962232722692910, 5.120942621315136556, 0.2927443173902372076 ) ) ;
#13493 = CARTESIAN_POINT ( 'NONE',  ( -0.2541070255160559066, 5.173678042950717426, -0.1516883682263707178 ) ) ;
#13494 = VECTOR ( 'NONE', #1607, 39.37007874015748143 ) ;
#13495 = CARTESIAN_POINT ( 'NONE',  ( -0.1292346314604057023, 4.790361111262843252, 0.3119999999999998885 ) ) ;
#13496 = CARTESIAN_POINT ( 'NONE',  ( -0.1993543840281266355, 4.929250000075866112, 0.1993543840281267465 ) ) ;
#13497 = ORIENTED_EDGE ( 'NONE', *, *, #20764, .F. ) ;
#13498 = CARTESIAN_POINT ( 'NONE',  ( -0.1167790944451423257, 4.231333333409199149, -0.2819296736111110424 ) ) ;
#13499 = ORIENTED_EDGE ( 'NONE', *, *, #13222, .T. ) ;
#13500 = CARTESIAN_POINT ( 'NONE',  ( 0.3613381517857143232, 0.1401785713310289838, -0.1174058825155740587 ) ) ;
#13501 = ADVANCED_FACE ( 'NONE', ( #23308 ), #1254, .T. ) ;
#13502 = EDGE_LOOP ( 'NONE', ( #21106, #5360, #2271, #16623 ) ) ;
#13503 = CC_DESIGN_APPROVAL ( #6729, ( #15678 ) ) ;
#13504 = ORIENTED_EDGE ( 'NONE', *, *, #15332, .F. ) ;
#13505 = PERSON_AND_ORGANIZATION ( #15518, #2538 ) ;
#13506 = CARTESIAN_POINT ( 'NONE',  ( -0.3155070326520293400, -0.1306872919485614626, 0.4025694444444489761 ) ) ;
#13507 = CARTESIAN_POINT ( 'NONE',  ( 0.5097595264191665532, 2.291712385858714285, -0.6667552972947643486 ) ) ;
#13508 = CARTESIAN_POINT ( 'NONE',  ( -0.1993543840281266910, 3.859805555631421470, -0.1993543840281266910 ) ) ;
#13509 = AXIS2_PLACEMENT_3D ( 'NONE', #3316, #22093, #10890 ) ;
#13510 = CARTESIAN_POINT ( 'NONE',  ( 0.3140227130263654187, 4.419434873055135604, -0.01898951124202318680 ) ) ;
#13511 = CARTESIAN_POINT ( 'NONE',  ( -0.4687500000000003886, -0.2598076211353319009, 0.3779506566538942125 ) ) ;
#13512 = FACE_OUTER_BOUND ( 'NONE', #21714, .T. ) ;
#13513 = CARTESIAN_POINT ( 'NONE',  ( 0.1954553509668047195, 0.1954553509668046085, 0.2897222222222257115 ) ) ;
#13514 = CARTESIAN_POINT ( 'NONE',  ( 1.726321361862525858E-17, 0.5076388888130222155, -0.2819296736111110979 ) ) ;
#13515 = CARTESIAN_POINT ( 'NONE',  ( -3.385114897866767815E-17, -0.2764156081756484196, 0.4425000000000046119 ) ) ;
#13516 = VERTEX_POINT ( 'NONE', #6615 ) ;
#13517 = CARTESIAN_POINT ( 'NONE',  ( -0.1993543840281266355, 4.707027777853643791, 0.1993543840281267465 ) ) ;
#13518 = CARTESIAN_POINT ( 'NONE',  ( -0.06335377612981497875, 0.4107590812887310094, -0.3999999999999999667 ) ) ;
#13519 = CARTESIAN_POINT ( 'NONE',  ( 0.1993543840281266633, 4.776472222298087544, -0.1993543840281266910 ) ) ;
#13520 = CARTESIAN_POINT ( 'NONE',  ( 3.887228417612631703E-07, 4.154944433789834690, -0.3119999999997578044 ) ) ;
#13521 =( BOUNDED_CURVE ( )  B_SPLINE_CURVE ( 2, ( #4709, #10337, #17763, #3009, #10460, #23348, #17886, #22723, #4066 ),
 .UNSPECIFIED., .F., .F. ) 
 B_SPLINE_CURVE_WITH_KNOTS ( ( 3, 2, 2, 2, 3 ),
 ( 0.3839285714285713969, 0.3883928571428570953, 0.3928571428571427937, 0.3973214285714284921, 0.4017857142857142461 ),
 .UNSPECIFIED. ) 
 CURVE ( )  GEOMETRIC_REPRESENTATION_ITEM ( )  RATIONAL_B_SPLINE_CURVE ( ( 1.000000000000000888, 0.9238795325112857393, 1.000000000000000000, 0.9238795325112867385, 1.000000000000000000, 0.9238795325112867385, 1.000000000000000000, 0.9238795325112877377, 0.9999999999999990008 ) ) 
 REPRESENTATION_ITEM ( '' )  );
#13522 = EDGE_CURVE ( 'NONE', #10074, #22264, #3889, .T. ) ;
#13523 = CARTESIAN_POINT ( 'NONE',  ( -0.04734746964375153438, 4.708926481085645203E-18, 0.3720189177726724306 ) ) ;
#13524 = CARTESIAN_POINT ( 'NONE',  ( 0.4593750000000003664, 0.2760455974562901482, 0.06112444011295366936 ) ) ;
#13525 = EDGE_CURVE ( 'NONE', #17212, #17737, #10530, .T. ) ;
#13526 = CARTESIAN_POINT ( 'NONE',  ( -0.2206173157302028232, 4.377166666666665762, -0.2206173157302028232 ) ) ;
#13527 = EDGE_CURVE ( 'NONE', #11401, #14964, #12488, .T. ) ;
#13528 = CARTESIAN_POINT ( 'NONE',  ( 0.2819296736111110979, 3.825083333409198705, -3.452642723725051716E-17 ) ) ;
#13529 = DIRECTION ( 'NONE',  ( 0.000000000000000000, -0.7071067811865475727, -0.7071067811865475727 ) ) ;
#13530 = ORIENTED_EDGE ( 'NONE', *, *, #20801, .T. ) ;
#13531 = CARTESIAN_POINT ( 'NONE',  ( 0.3053277220128169378, 4.587655388424375147, -0.07727936894157313996 ) ) ;
#13532 = ORIENTED_EDGE ( 'NONE', *, *, #12175, .F. ) ;
#13533 = EDGE_CURVE ( 'NONE', #18846, #409, #17523, .T. ) ;
#13534 = CARTESIAN_POINT ( 'NONE',  ( -1.296004783052830448E-07, 4.710500003633881327, -0.3119999999999730766 ) ) ;
#13535 = CARTESIAN_POINT ( 'NONE',  ( 0.002698052836345287992, 4.654867065270698490, -0.3119899994661654574 ) ) ;
#13536 = CARTESIAN_POINT ( 'NONE',  ( -0.1306872919485615459, -0.3155070326520293400, -0.1460416666666664309 ) ) ;
#13537 = LINE ( 'NONE', #23011, #20831 ) ;
#13538 = ORIENTED_EDGE ( 'NONE', *, *, #19811, .T. ) ;
#13539 = CARTESIAN_POINT ( 'NONE',  ( -0.3613381517857143232, 0.4008928570453146878, -0.1174058825155741004 ) ) ;
#13540 = AXIS2_PLACEMENT_3D ( 'NONE', #10301, #3323, #2841 ) ;
#13541 = CARTESIAN_POINT ( 'NONE',  ( -5.178964085587577574E-17, 0.4659722221463555858, 0.2819296736111110979 ) ) ;
#13542 = CARTESIAN_POINT ( 'NONE',  ( 0.08166507714107607008, 3.851613536341646160, 0.3038795024021940239 ) ) ;
#13543 = CARTESIAN_POINT ( 'NONE',  ( 0.1303878333502071496, 0.2053964056049825126, -1.229337499098527076 ) ) ;
#13544 = CARTESIAN_POINT ( 'NONE',  ( -0.2944048850341824952, -0.06890421275380248511, -0.09102616896780499345 ) ) ;
#13545 = CARTESIAN_POINT ( 'NONE',  ( 0.1954553509668047195, 0.1954553509668046085, 0.1300000000000021694 ) ) ;
#13546 = EDGE_LOOP ( 'NONE', ( #22836, #21063, #16164, #12264, #13173, #16068, #22364, #3414, #17614, #173, #22504 ) ) ;
#13547 = CARTESIAN_POINT ( 'NONE',  ( -0.2669838093744815177, 4.608413313809449185, -0.1638134789338530906 ) ) ;
#13548 = CARTESIAN_POINT ( 'NONE',  ( -0.5116234456863258950, 4.559812086079793048, -2.813986238491759551 ) ) ;
#13549 = CARTESIAN_POINT ( 'NONE',  ( -0.3124999999999997224, 0.1294417382415924966, 0.3418055555555596370 ) ) ;
#13550 = CARTESIAN_POINT ( 'NONE',  ( 0.2206173157302028232, 0.1361111111111107663, -0.2206173157302028232 ) ) ;
#13551 = CARTESIAN_POINT ( 'NONE',  ( -0.2206173157302028232, 5.154944444444443441, -0.2206173157302028232 ) ) ;
#13552 = CARTESIAN_POINT ( 'NONE',  ( -0.2819296736111110424, 4.196611111186976828, -0.1167790944451423119 ) ) ;
#13553 = DIRECTION ( 'NONE',  ( -0.5773502691896257311, -0.5773502691896257311, 0.5773502691896258421 ) ) ;
#13554 = CARTESIAN_POINT ( 'NONE',  ( 0.3228432657101673042, 2.690047770615767941, -1.025353588051019837 ) ) ;
#13555 = CARTESIAN_POINT ( 'NONE',  ( -0.3253415854805812857, 3.738758431839877614E-19, -0.1145082521472477743 ) ) ;
#13556 = ORIENTED_EDGE ( 'NONE', *, *, #1913, .F. ) ;
#13557 = EDGE_LOOP ( 'NONE', ( #3104, #7609, #10438, #105, #527 ) ) ;
#13558 = CARTESIAN_POINT ( 'NONE',  ( 1.750236327630675475E-17, 0.3374999998049151295, -0.3999999999999999667 ) ) ;
#13559 = ADVANCED_FACE ( 'NONE', ( #8570 ), #16011, .T. ) ;
#13560 = CARTESIAN_POINT ( 'NONE',  ( 0.1167790944451422702, 4.835500000075865223, -0.2819296736111110424 ) ) ;
#13561 = CARTESIAN_POINT ( 'NONE',  ( -0.2998642343065030524, 0.08796414601291394075, -0.1016666666666771329 ) ) ;
#13562 = CARTESIAN_POINT ( 'NONE',  ( -0.07787416272928887606, 5.165394585812085992, 0.2883211566397950176 ) ) ;
#13563 = TOROIDAL_SURFACE ( 'NONE', #8867, 0.3425000000000000266, 0.02999999999999999889 ) ;
#13564 =( BOUNDED_CURVE ( )  B_SPLINE_CURVE ( 2, ( #21344, #3279, #974, #17805, #1459, #1337, #2802, #10611, #8766 ),
 .UNSPECIFIED., .F., .F. ) 
 B_SPLINE_CURVE_WITH_KNOTS ( ( 3, 2, 2, 2, 3 ),
 ( 0.06250000000000002776, 0.07291666666666669905, 0.08333333333333335646, 0.09375000000000002776, 0.1041666666666666990 ),
 .UNSPECIFIED. ) 
 CURVE ( )  GEOMETRIC_REPRESENTATION_ITEM ( )  RATIONAL_B_SPLINE_CURVE ( ( 0.9999999999999997780, 0.9238795325112869605, 1.000000000000000000, 0.9238795325112867385, 1.000000000000000000, 0.9238795325112867385, 1.000000000000000000, 0.9238795325112865164, 1.000000000000000222 ) ) 
 REPRESENTATION_ITEM ( '' )  );
#13565 = APPROVAL_DATE_TIME ( #11973, #14786 ) ;
#13566 = CARTESIAN_POINT ( 'NONE',  ( 0.01571813568754789822, 3.710075998628030725, -0.3116604989128209935 ) ) ;
#13567 = DIRECTION ( 'NONE',  ( 0.000000000000000000, 0.000000000000000000, -1.000000000000000000 ) ) ;
#13568 = CARTESIAN_POINT ( 'NONE',  ( -0.2819296736111110424, 4.370222222298088433, 0.1167790944451424923 ) ) ;
#13569 = APPROVAL_DATE_TIME ( #4032, #619 ) ;
#13570 = CARTESIAN_POINT ( 'NONE',  ( -0.2827572605903787006, 4.061666605139203412, 0.1376332577019660497 ) ) ;
#13571 = CARTESIAN_POINT ( 'NONE',  ( 0.7919466436700954848, 2.665000000000000036, -2.986000000000000210 ) ) ;
#13572 = DIRECTION ( 'NONE',  ( 0.000000000000000000, 0.000000000000000000, -1.000000000000000000 ) ) ;
#13573 = CARTESIAN_POINT ( 'NONE',  ( -0.1993543840281266633, 0.3479166665908000611, -0.1993543840281266910 ) ) ;
#13574 = DIRECTION ( 'NONE',  ( -0.000000000000000000, -1.000000000000000000, -0.000000000000000000 ) ) ;
#13575 = CARTESIAN_POINT ( 'NONE',  ( -0.3798103452830965954, 0.002729592702593379612, 0.1577565542260639386 ) ) ;
#13576 = CARTESIAN_POINT ( 'NONE',  ( -3.863846776457871776E-17, -0.3155070326520292845, 0.1872916666666691043 ) ) ;
#13577 = CARTESIAN_POINT ( 'NONE',  ( -0.5116234456863258950, 4.111524471938507119, -3.001780280100677434 ) ) ;
#13578 = CARTESIAN_POINT ( 'NONE',  ( -0.4749999999999999778, 3.575000000000000622, -0.09499999999999995948 ) ) ;
#13579 = CARTESIAN_POINT ( 'NONE',  ( 0.1167790944451423535, 0.4138888888130222155, 0.2819296736111110979 ) ) ;
#13580 = CARTESIAN_POINT ( 'NONE',  ( -0.2819296736111110979, 0.1222222221463555719, 0.1167790944451422425 ) ) ;
#13581 = CARTESIAN_POINT ( 'NONE',  ( 0.1993543840281267465, 4.276472222298088433, 0.1993543840281266633 ) ) ;
#13582 = VECTOR ( 'NONE', #24061, 39.37007874015748143 ) ;
#13583 = CARTESIAN_POINT ( 'NONE',  ( -0.3236067977499790249, 0.2196428569477723303, 0.2351141009169892271 ) ) ;
#13584 = CARTESIAN_POINT ( 'NONE',  ( 0.1993543840281267465, 4.943138888964754507, 0.1993543840281266633 ) ) ;
#13585 = CARTESIAN_POINT ( 'NONE',  ( -1.726321361862525858E-17, 4.116750000075865223, -0.2819296736111110979 ) ) ;
#13586 = DIRECTION ( 'NONE',  ( -0.000000000000000000, -1.000000000000000000, -0.000000000000000000 ) ) ;
#13587 = EDGE_LOOP ( 'NONE', ( #9826, #19205, #12600, #12637, #6888, #2153, #9373 ) ) ;
#13588 = CARTESIAN_POINT ( 'NONE',  ( 0.3120000000000000551, 4.519527777777776478, 0.1292346314604056190 ) ) ;
#13589 = CARTESIAN_POINT ( 'NONE',  ( -0.3119999999999998885, 3.950083333485065573, 0.1292346314604058410 ) ) ;
#13590 = CARTESIAN_POINT ( 'NONE',  ( -0.1578986201652095300, 0.4501030665082202953, 0.4142710792078266313 ) ) ;
#13591 = DIRECTION ( 'NONE',  ( 1.000000000000000000, 0.000000000000000000, 0.000000000000000000 ) ) ;
#13592 = CIRCLE ( 'NONE', #16692, 0.2500000000000000000 ) ;
#13593 = CALENDAR_DATE ( 2026, 7, 10 ) ;
#13594 = CARTESIAN_POINT ( 'NONE',  ( 2.316810681416314743, 2.319533376497107557, -2.476240473580834323 ) ) ;
#13595 = CARTESIAN_POINT ( 'NONE',  ( -0.2228772273359933276, 5.009026790445733290, 0.2183502748428790829 ) ) ;
#13596 = EDGE_LOOP ( 'NONE', ( #5883, #15462, #2988, #11393 ) ) ;
#13597 = CARTESIAN_POINT ( 'NONE',  ( 0.2819296736111110424, -0.002777777853644406401, -0.1167790944451423119 ) ) ;
#13598 = EDGE_LOOP ( 'NONE', ( #1470, #16636, #10474, #21005 ) ) ;
#13599 = CARTESIAN_POINT ( 'NONE',  ( 0.2846063461394666150, 4.255906380294286251, -0.1278434303317485254 ) ) ;
#13600 = CARTESIAN_POINT ( 'NONE',  ( 0.2725502669324571525, 0.3839089073841462363, 0.4290249205314688452 ) ) ;
#13601 = FACE_OUTER_BOUND ( 'NONE', #12877, .T. ) ;
#13602 = CARTESIAN_POINT ( 'NONE',  ( -0.2233192592356399997, 0.04017857133102901990, 0.3073725909049499494 ) ) ;
#13603 = CARTESIAN_POINT ( 'NONE',  ( 0.07617771740037646011, 5.188451671420351907, -0.2803169692743197605 ) ) ;
#13604 = ORIENTED_EDGE ( 'NONE', *, *, #22118, .F. ) ;
#13605 = CARTESIAN_POINT ( 'NONE',  ( 0.3613381517857143232, 0.3008928570453147100, -0.1174058825155740587 ) ) ;
#13606 = DIRECTION ( 'NONE',  ( -0.000000000000000000, 0.000000000000000000, -1.000000000000000000 ) ) ;
#13607 = CARTESIAN_POINT ( 'NONE',  ( -0.03922894998300566205, 4.681526571591189345, 0.3120000079934041604 ) ) ;
#13608 = APPROVAL ( #16003, 'UNSPECIFIED' ) ;
#13609 = CARTESIAN_POINT ( 'NONE',  ( 0.1167790944451424368, 4.036888888964754507, 0.2819296736111110424 ) ) ;
#13610 = CARTESIAN_POINT ( 'NONE',  ( 0.8977114317029943891, 2.978485840173427324, -0.6898620042323803103 ) ) ;
#13611 = CARTESIAN_POINT ( 'NONE',  ( -0.1031275500757723590, 5.166304435049627664, -0.2794537332880138725 ) ) ;
#13612 = CARTESIAN_POINT ( 'NONE',  ( -0.1292346314604056745, 4.436194444596177178, -0.3119999999999999996 ) ) ;
#13613 = CARTESIAN_POINT ( 'NONE',  ( -0.1993543840281266355, 4.873694444520310753, 0.1993543840281267465 ) ) ;
#13614 = VERTEX_POINT ( 'NONE', #14181 ) ;
#13615 = CARTESIAN_POINT ( 'NONE',  ( 0.1167790944451422702, 4.224388888964755395, -0.2819296736111110424 ) ) ;
#13616 = ORIENTED_EDGE ( 'NONE', *, *, #8365, .T. ) ;
#13617 = CARTESIAN_POINT ( 'NONE',  ( 0.2233192592356400275, 0.2901785713310290338, -0.3073725909049499494 ) ) ;
#13618 = VERTEX_POINT ( 'NONE', #19909 ) ;
#13619 = ORIENTED_EDGE ( 'NONE', *, *, #15409, .T. ) ;
#13620 = DATE_TIME_ROLE ( 'creation_date' ) ;
#13621 = CARTESIAN_POINT ( 'NONE',  ( 0.3255746763033851021, 3.686631053841027850, -0.09499999999999995948 ) ) ;
#13622 = DIRECTION ( 'NONE',  ( 0.000000000000000000, 0.000000000000000000, -1.000000000000000000 ) ) ;
#13623 = CARTESIAN_POINT ( 'NONE',  ( 0.01848103877824584448, 0.5441716683897389606, 0.04413116910601658227 ) ) ;
#13624 = AXIS2_PLACEMENT_3D ( 'NONE', #1210, #6814, #14257 ) ;
#13625 = ADVANCED_FACE ( 'NONE', ( #1135 ), #11485, .T. ) ;
#13626 = CARTESIAN_POINT ( 'NONE',  ( 0.1081575060082094752, 4.408054576103176636, 0.2929456441888016460 ) ) ;
#13627 = CARTESIAN_POINT ( 'NONE',  ( 0.3125000000000000000, -5.740531871003217465E-17, 0.2619444444444478659 ) ) ;
#13628 = DIRECTION ( 'NONE',  ( -0.8660254037844397068, -1.060575238724908024E-16, -0.4999999999999979461 ) ) ;
#13629 = CARTESIAN_POINT ( 'NONE',  ( -0.2764156081756484196, 1.692557448933383907E-17, 0.1994444444444472553 ) ) ;
#13630 = CARTESIAN_POINT ( 'NONE',  ( 0.2819296736111110979, 0.5493055554796889561, 0.000000000000000000 ) ) ;
#13631 = CARTESIAN_POINT ( 'NONE',  ( -0.2764156081756484196, -0.1144950937579609362, 0.3765277777777819579 ) ) ;
#13632 = ORIENTED_EDGE ( 'NONE', *, *, #14082, .T. ) ;
#13633 = CARTESIAN_POINT ( 'NONE',  ( 0.1167790944451424368, 4.773000000075866112, 0.2819296736111110424 ) ) ;
#13634 = CARTESIAN_POINT ( 'NONE',  ( 0.01848103877824608041, -0.5441716683897390716, 0.04413116910601659615 ) ) ;
#13635 = ADVANCED_FACE ( 'NONE', ( #23365 ), #23482, .T. ) ;
#13636 = CARTESIAN_POINT ( 'NONE',  ( -0.1993543840281266910, 4.734805555631420582, -0.1993543840281266910 ) ) ;
#13637 = CARTESIAN_POINT ( 'NONE',  ( -0.02540882200436479776, 4.155671449734249734, -0.3110052518984787739 ) ) ;
#13638 = CARTESIAN_POINT ( 'NONE',  ( 0.1409648704857156543, 4.853596617052923001, 0.2789902241728853260 ) ) ;
#13639 = LINE ( 'NONE', #2529, #23832 ) ;
#13640 = CARTESIAN_POINT ( 'NONE',  ( 0.000000000000000000, 0.8949999999999999067, 0.000000000000000000 ) ) ;
#13641 = CARTESIAN_POINT ( 'NONE',  ( 0.3119999999999999996, 4.186194444444444329, 0.1292346314604056190 ) ) ;
#13642 = CARTESIAN_POINT ( 'NONE',  ( -0.1993543840281266910, 3.790361111186976828, -0.1993543840281266910 ) ) ;
#13643 = DIRECTION ( 'NONE',  ( 0.000000000000000000, 0.000000000000000000, 1.000000000000000000 ) ) ;
#13644 = AXIS2_PLACEMENT_3D ( 'NONE', #18830, #19185, #5898 ) ;
#13645 = ORIENTED_EDGE ( 'NONE', *, *, #20732, .T. ) ;
#13646 = CARTESIAN_POINT ( 'NONE',  ( 0.3104769350984191711, 4.584653674997469786, 0.03084955884225352996 ) ) ;
#13647 = ORIENTED_EDGE ( 'NONE', *, *, #19318, .T. ) ;
#13648 = CARTESIAN_POINT ( 'NONE',  ( 0.2859729506740118499, 4.700254050761267344, -0.1247996014322190345 ) ) ;
#13649 = UNCERTAINTY_MEASURE_WITH_UNIT (LENGTH_MEASURE( 1.000000000000000082E-05 ), #18664, 'distance_accuracy_value', 'NONE');
#13650 = DIRECTION ( 'NONE',  ( 0.000000000000000000, 1.000000000000000000, 0.000000000000000000 ) ) ;
#13651 = EDGE_CURVE ( 'NONE', #17792, #13125, #17162, .T. ) ;
#13652 = CARTESIAN_POINT ( 'NONE',  ( -0.1954553509668046918, -0.1954553509668046640, 0.4286111111111157168 ) ) ;
#13653 = EDGE_CURVE ( 'NONE', #14487, #8144, #19365, .T. ) ;
#13654 = CARTESIAN_POINT ( 'NONE',  ( 1.573500000000000343, -3.414809992080329023E-17, -0.3524999999999999800 ) ) ;
#13655 = ORIENTED_EDGE ( 'NONE', *, *, #12032, .T. ) ;
#13656 =( BOUNDED_CURVE ( )  B_SPLINE_CURVE ( 2, ( #3640, #20109, #16092, #1574, #21926, #7306, #9129, #8891, #9012 ),
 .UNSPECIFIED., .F., .F. ) 
 B_SPLINE_CURVE_WITH_KNOTS ( ( 3, 2, 2, 2, 3 ),
 ( 0.1500366067892652533, 0.1562500000000000000, 0.1666666666666666574, 0.1770833333333333426, 0.1875000000000000000 ),
 .UNSPECIFIED. ) 
 CURVE ( )  GEOMETRIC_REPRESENTATION_ITEM ( )  RATIONAL_B_SPLINE_CURVE ( ( 0.9633570531806863180, 0.9545952259943366602, 1.000000000000000000, 0.9238795325112867385, 1.000000000000000000, 0.9238795325112867385, 1.000000000000000000, 0.9238795325112867385, 1.000000000000000000 ) ) 
 REPRESENTATION_ITEM ( '' )  );
#13657 = CARTESIAN_POINT ( 'NONE',  ( 0.3613381517857143232, -0.07410714295468522061, -0.1174058825155740587 ) ) ;
#13658 = VECTOR ( 'NONE', #13063, 39.37007874015748854 ) ;
#13659 = CARTESIAN_POINT ( 'NONE',  ( 0.1167790944451423535, 0.5249999999241333759, 0.2819296736111110424 ) ) ;
#13660 = FACE_OUTER_BOUND ( 'NONE', #7607, .T. ) ;
#13661 = CARTESIAN_POINT ( 'NONE',  ( 0.2472135954999579721, 0.04464285694777234831, -0.3402603233408160732 ) ) ;
#13662 = CARTESIAN_POINT ( 'NONE',  ( 2.319244702705235195, 2.291712385858714729, -2.476240473580834323 ) ) ;
#13663 = CARTESIAN_POINT ( 'NONE',  ( 0.2764156081756484196, -5.077672346800151106E-17, 0.2341666666666696595 ) ) ;
#13664 = ADVANCED_FACE ( 'NONE', ( #21316 ), #1068, .T. ) ;
#13665 = EDGE_LOOP ( 'NONE', ( #20727, #16252, #6249, #8597, #13619 ) ) ;
#13666 = CARTESIAN_POINT ( 'NONE',  ( -0.1582747645997409358, 4.622434822458711068, 0.2689245564580552972 ) ) ;
#13667 = CARTESIAN_POINT ( 'NONE',  ( 0.06335377612981456241, 0.08933050986015969586, 0.3999999999999999667 ) ) ;
#13668 = CARTESIAN_POINT ( 'NONE',  ( 0.2320196243301847205, 1.046010598739759003E-17, -0.2860823100163923383 ) ) ;
#13669 = CARTESIAN_POINT ( 'NONE',  ( -0.1292346314604056190, 0.2576388888888885287, -0.3119999999999999996 ) ) ;
#13670 = CARTESIAN_POINT ( 'NONE',  ( 5.731347020009612645E-17, 4.953555555555554157, 0.3119999999999999996 ) ) ;
#13671 = CARTESIAN_POINT ( 'NONE',  ( -1.726321361862525858E-17, 4.075083333409199149, -0.2819296736111110979 ) ) ;
#13672 = CARTESIAN_POINT ( 'NONE',  ( -0.1916416111016578661, 4.343568013825621854, 0.2495666673098946020 ) ) ;
#13673 = DIRECTION ( 'NONE',  ( -0.000000000000000000, 1.000000000000000000, -0.000000000000000000 ) ) ;
#13674 = CARTESIAN_POINT ( 'NONE',  ( 0.3601051986570594221, -1.207678508861135529E-18, 0.03795131042432794977 ) ) ;
#13675 = VERTEX_POINT ( 'NONE', #12305 ) ;
#13676 = ORIENTED_EDGE ( 'NONE', *, *, #22775, .T. ) ;
#13677 = CARTESIAN_POINT ( 'NONE',  ( -0.4739766090219371120, -0.2774257203002796213, 0.04193793378272819145 ) ) ;
#13678 = CARTESIAN_POINT ( 'NONE',  ( -0.2819296736111110424, 4.745222222298088433, 0.1167790944451424923 ) ) ;
#13679 = CARTESIAN_POINT ( 'NONE',  ( 0.3613381517857143232, 0.3544642856167432576, -0.1174058825155740587 ) ) ;
#13680 = AXIS2_PLACEMENT_3D ( 'NONE', #6055, #15571, #18870 ) ;
#13681 = CARTESIAN_POINT ( 'NONE',  ( -0.2206173157302028232, 4.099388888888888083, -0.2206173157302028232 ) ) ;
#13682 = AXIS2_PLACEMENT_3D ( 'NONE', #1774, #22257, #13960 ) ;
#13683 = CALENDAR_DATE ( 2026, 7, 10 ) ;
#13684 = DIRECTION ( 'NONE',  ( -0.000000000000000000, -1.000000000000000000, -0.000000000000000000 ) ) ;
#13685 = CARTESIAN_POINT ( 'NONE',  ( -1.726321361862525858E-17, 4.352861111186976828, -0.2819296736111110979 ) ) ;
#13686 = LINE ( 'NONE', #21103, #815 ) ;
#13687 = DIRECTION ( 'NONE',  ( 0.000000000000000000, 0.000000000000000000, -1.000000000000000000 ) ) ;
#13688 = DIRECTION ( 'NONE',  ( 0.8320502943378439431, -0.4803844614152621428, -0.2773500981126125753 ) ) ;
#13689 = CARTESIAN_POINT ( 'NONE',  ( -0.1993543840281266633, 0.4034722221463555858, -0.1993543840281266910 ) ) ;
#13690 = DIRECTION ( 'NONE',  ( 0.8660254037844443697, 0.000000000000000000, -0.4999999999999901745 ) ) ;
#13691 = CARTESIAN_POINT ( 'NONE',  ( -0.4000000000000000222, 0.1535714285714285254, 0.1299678784931624920 ) ) ;
#13692 = DIRECTION ( 'NONE',  ( 0.4999999999999941158, 0.000000000000000000, 0.8660254037844420383 ) ) ;
#13693 = CARTESIAN_POINT ( 'NONE',  ( -0.3155070326520293400, -0.1306872919485614626, 0.2324305555555583602 ) ) ;
#13694 = EDGE_CURVE ( 'NONE', #6119, #7025, #13065, .T. ) ;
#13695 = PLANE ( 'NONE',  #19610 ) ;
#13696 = DIRECTION ( 'NONE',  ( 0.7071067811865451302, -0.06162841671621964446, -0.7044160264027610197 ) ) ;
#13697 = CARTESIAN_POINT ( 'NONE',  ( -5.178964085587577574E-17, 0.4104166665908000056, 0.2819296736111110979 ) ) ;
#13698 = CARTESIAN_POINT ( 'NONE',  ( 0.1993543840281266355, 0.1395833332574667185, 0.1993543840281267465 ) ) ;
#13699 = AXIS2_PLACEMENT_3D ( 'NONE', #1327, #18273, #12933 ) ;
#13700 = CARTESIAN_POINT ( 'NONE',  ( -0.1167790944451423535, 4.043833333409200037, 0.2819296736111110424 ) ) ;
#13701 = CARTESIAN_POINT ( 'NONE',  ( 0.3236067977499789694, 0.3839285712334866152, 0.2351141009169893659 ) ) ;
#13702 = CARTESIAN_POINT ( 'NONE',  ( 0.1167790944451422702, 4.849388888964755395, -0.2819296736111110424 ) ) ;
#13703 = CARTESIAN_POINT ( 'NONE',  ( 0.1292346314604056745, 0.4104166665149337478, -0.3119999999999999996 ) ) ;
#13704 = ORIENTED_EDGE ( 'NONE', *, *, #23443, .T. ) ;
#13705 = CYLINDRICAL_SURFACE ( 'NONE', #8557, 0.3119999999999999996 ) ;
#13706 = CARTESIAN_POINT ( 'NONE',  ( -0.1292346314604057023, 3.901472222373954857, 0.3119999999999998885 ) ) ;
#13707 = CARTESIAN_POINT ( 'NONE',  ( 2.159030003005114828, 2.291712385858714285, -2.568740473580834127 ) ) ;
#13708 =( NAMED_UNIT ( * ) SI_UNIT ( $, .STERADIAN. ) SOLID_ANGLE_UNIT ( ) );
#13709 = ORIENTED_EDGE ( 'NONE', *, *, #15962, .F. ) ;
#13710 = APPROVAL_DATE_TIME ( #3080, #13608 ) ;
#13711 = CARTESIAN_POINT ( 'NONE',  ( 0.3236067977499790249, 0.3357142857142856318, -0.2351141009169892826 ) ) ;
#13712 = CARTESIAN_POINT ( 'NONE',  ( -0.5116234456863258950, 4.901168349308694161, -2.640781157734872320 ) ) ;
#13713 = VERTEX_POINT ( 'NONE', #19823 ) ;
#13714 = CARTESIAN_POINT ( 'NONE',  ( 0.1993543840281266910, 0.05624999992413336897, -0.1993543840281266910 ) ) ;
#13715 = EDGE_LOOP ( 'NONE', ( #20344, #2027 ) ) ;
#13716 = CARTESIAN_POINT ( 'NONE',  ( -0.2472135954999579999, 0.01785714285714282493, 0.3402603233408160732 ) ) ;
#13717 = CARTESIAN_POINT ( 'NONE',  ( 0.4622078388679875527, 0.2744100571732868143, 0.3892820121258429023 ) ) ;
#13718 = CARTESIAN_POINT ( 'NONE',  ( 0.04915613994164541589, 4.073065570104705380, 0.3089926667392805526 ) ) ;
#13719 = CARTESIAN_POINT ( 'NONE',  ( -0.2233192592356399997, 0.3258928570453145657, 0.3073725909049499494 ) ) ;
#13720 = FACE_OUTER_BOUND ( 'NONE', #16106, .T. ) ;
#13721 = EDGE_LOOP ( 'NONE', ( #21471, #18196, #2854, #3712 ) ) ;
#13722 = CARTESIAN_POINT ( 'NONE',  ( 2.326421213736078119E-17, 0.3151785713310290005, -0.3799334167787516980 ) ) ;
#13723 = DIRECTION ( 'NONE',  ( 0.000000000000000000, 0.000000000000000000, -1.000000000000000000 ) ) ;
#13724 = CARTESIAN_POINT ( 'NONE',  ( 0.1167790944451422702, 3.946611111186976384, -0.2819296736111110424 ) ) ;
#13725 = DIRECTION ( 'NONE',  ( 0.000000000000000000, 0.000000000000000000, 1.000000000000000000 ) ) ;
#13726 = CARTESIAN_POINT ( 'NONE',  ( -0.01909785675588383455, 5.196999109626997182, 0.2863020908690515620 ) ) ;
#13727 = CARTESIAN_POINT ( 'NONE',  ( -0.2206173157302028232, 4.606333333485065573, -0.2206173157302028232 ) ) ;
#13728 = CARTESIAN_POINT ( 'NONE',  ( 0.2819296736111110979, 4.842444444520309865, -0.1167790944451423396 ) ) ;
#13729 = ORIENTED_EDGE ( 'NONE', *, *, #18869, .T. ) ;
#13730 = CARTESIAN_POINT ( 'NONE',  ( 5.178964085587577574E-17, 3.977861111186976384, 0.2819296736111110979 ) ) ;
#13731 = CARTESIAN_POINT ( 'NONE',  ( -0.2233192592356400275, 0.2544642856167432798, 0.3073725909049499494 ) ) ;
#13732 = EDGE_LOOP ( 'NONE', ( #19181, #1646, #675, #2812 ) ) ;
#13733 = VERTEX_POINT ( 'NONE', #19573 ) ;
#13734 = PERSON_AND_ORGANIZATION_ROLE ( 'design_supplier' ) ;
#13735 = VERTEX_POINT ( 'NONE', #19698 ) ;
#13736 = CARTESIAN_POINT ( 'NONE',  ( -0.2694453590030796430, -0.3748737188716306790, 0.4343212420608418278 ) ) ;
#13737 = CARTESIAN_POINT ( 'NONE',  ( 0.000000000000000000, 0.4987679491924311148, 0.000000000000000000 ) ) ;
#13738 = CARTESIAN_POINT ( 'NONE',  ( -5.731347020009612645E-17, 0.05277777762604484585, 0.3119999999999999996 ) ) ;
#13739 = CARTESIAN_POINT ( 'NONE',  ( 0.2629417729398952353, 5.140591734628677578, 0.1550161288497664824 ) ) ;
#13740 = CARTESIAN_POINT ( 'NONE',  ( 0.2206173157302027676, 0.1708333331816004053, 0.2206173157302028787 ) ) ;
#13741 = DIRECTION ( 'NONE',  ( 0.000000000000000000, 0.000000000000000000, -1.000000000000000000 ) ) ;
#13742 = CARTESIAN_POINT ( 'NONE',  ( 0.09694982473845883963, 0.06249891840240667101, 0.2965547697865978938 ) ) ;
#13743 = CARTESIAN_POINT ( 'NONE',  ( -0.1954553509668046918, -0.1954553509668046640, 0.1508333333333357063 ) ) ;
#13744 = CARTESIAN_POINT ( 'NONE',  ( -0.2819296736111110979, 0.1152777777019111383, -0.1167790944451423396 ) ) ;
#13745 = CARTESIAN_POINT ( 'NONE',  ( 0.1144950937579611444, 0.2764156081756483641, 0.4668055555555604141 ) ) ;
#13746 = CARTESIAN_POINT ( 'NONE',  ( 0.2819296736111110424, 4.786888888964755395, -0.1167790944451423396 ) ) ;
#13747 = FACE_OUTER_BOUND ( 'NONE', #22840, .T. ) ;
#13748 = VECTOR ( 'NONE', #4727, 39.37007874015748143 ) ;
#13749 = CARTESIAN_POINT ( 'NONE',  ( -0.1993543840281266355, 4.748694444520309865, 0.1993543840281267465 ) ) ;
#13750 = CARTESIAN_POINT ( 'NONE',  ( -0.1002000441541520542, 4.157805295584717342, -0.2961774115687041964 ) ) ;
#13751 = CARTESIAN_POINT ( 'NONE',  ( 0.1851001322554625683, 4.855041628199087356, 0.2517309871580742375 ) ) ;
#13752 = CARTESIAN_POINT ( 'NONE',  ( 0.000000000000000000, 5.384999999999999787, 0.000000000000000000 ) ) ;
#13753 = CARTESIAN_POINT ( 'NONE',  ( 0.000000000000000000, 0.1199999999999999956, -0.3150000000000000022 ) ) ;
#13754 = CARTESIAN_POINT ( 'NONE',  ( 5.731347020009612645E-17, 4.231333333333332725, 0.3119999999999999996 ) ) ;
#13755 = CARTESIAN_POINT ( 'NONE',  ( 0.3119999999999999996, 5.196611111262844140, -3.820898013339742174E-17 ) ) ;
#13756 = CARTESIAN_POINT ( 'NONE',  ( 0.2905230268857740272, 4.971080770670708304, 0.1149655184485972731 ) ) ;
#13757 = ORIENTED_EDGE ( 'NONE', *, *, #165, .F. ) ;
#13758 = DIRECTION ( 'NONE',  ( -0.8660254037844434816, 0.000000000000000000, -0.4999999999999913403 ) ) ;
#13759 = ORIENTED_EDGE ( 'NONE', *, *, #19301, .T. ) ;
#13760 = CARTESIAN_POINT ( 'NONE',  ( 0.02915501805629885923, 4.709709316167313808, -0.3107256135361845528 ) ) ;
#13761 = AXIS2_PLACEMENT_3D ( 'NONE', #11505, #8067, #11381 ) ;
#13762 = ADVANCED_FACE ( 'NONE', ( #15685, #14097 ), #4814, .F. ) ;
#13763 = FACE_OUTER_BOUND ( 'NONE', #11278, .T. ) ;
#13764 = CARTESIAN_POINT ( 'NONE',  ( -0.3155070326520293400, -0.1306872919485614626, 0.1247916666666690211 ) ) ;
#13765 = CARTESIAN_POINT ( 'NONE',  ( 1.573500000000000343, 0.05625000000000004996, -1.412500000000000089 ) ) ;
#13766 = CARTESIAN_POINT ( 'NONE',  ( 0.1116596296178199860, 0.07946428561674331870, -0.3436530038418508792 ) ) ;
#13767 = CARTESIAN_POINT ( 'NONE',  ( -0.1993543840281266633, 0.4451388888130222710, -0.1993543840281266910 ) ) ;
#13768 = CARTESIAN_POINT ( 'NONE',  ( -0.1486148644933975860, 5.206640035683666845, 0.2403663825195851700 ) ) ;
#13769 = CARTESIAN_POINT ( 'NONE',  ( 0.2923287055106771337, 0.004464285616743319737, 0.2123892367102621359 ) ) ;
#13770 = PLANE ( 'NONE',  #7431 ) ;
#13771 = CARTESIAN_POINT ( 'NONE',  ( 9.001153973733040933E-17, 3.700000000000000622, 0.7199999999999994182 ) ) ;
#13772 = EDGE_LOOP ( 'NONE', ( #7319, #22946, #1289, #2509 ) ) ;
#13773 = CARTESIAN_POINT ( 'NONE',  ( -0.1500997534610212791, 4.622705627101820980, 0.2735216599064862475 ) ) ;
#13774 = DIRECTION ( 'NONE',  ( 0.000000000000000000, -0.000000000000000000, 1.000000000000000000 ) ) ;
#13775 = CARTESIAN_POINT ( 'NONE',  ( -0.1294417382415922191, 0.3125000000000000000, 0.3348611111111151617 ) ) ;
#13776 = CARTESIAN_POINT ( 'NONE',  ( 0.1292346314604056745, 0.4729166666666663188, -0.3119999999999999996 ) ) ;
#13777 = CARTESIAN_POINT ( 'NONE',  ( 0.2206173157302028787, 4.849388888888888083, 0.2206173157302027954 ) ) ;
#13778 = CARTESIAN_POINT ( 'NONE',  ( 0.1993543840281267465, 3.943138888964754951, 0.1993543840281266633 ) ) ;
#13779 = CARTESIAN_POINT ( 'NONE',  ( -0.1292346314604057300, 3.838972222222221564, 0.3119999999999998885 ) ) ;
#13780 = CARTESIAN_POINT ( 'NONE',  ( 0.009375000000000067307, -0.5358532185916218271, 0.06112444011295370405 ) ) ;
#13781 = CARTESIAN_POINT ( 'NONE',  ( 0.3178873086046067331, 2.458266394542412200E-17, 0.1722007902088446563 ) ) ;
#13782 = ORIENTED_EDGE ( 'NONE', *, *, #11390, .T. ) ;
#13783 = ADVANCED_FACE ( 'NONE', ( #17999 ), #21432, .F. ) ;
#13784 = ORIENTED_EDGE ( 'NONE', *, *, #8297, .F. ) ;
#13785 = EDGE_CURVE ( 'NONE', #21724, #13860, #7412, .T. ) ;
#13786 = CARTESIAN_POINT ( 'NONE',  ( 0.000000000000000000, 5.384999999999999787, -0.3119999999999999996 ) ) ;
#13787 = CARTESIAN_POINT ( 'NONE',  ( 5.178964085587577574E-17, 4.811194444520309865, 0.2819296736111110979 ) ) ;
#13788 = PLANE ( 'NONE',  #7966 ) ;
#13789 = ADVANCED_FACE ( 'NONE', ( #2866 ), #920, .T. ) ;
#13790 = PERSON_AND_ORGANIZATION_ROLE ( 'creator' ) ;
#13791 = CARTESIAN_POINT ( 'NONE',  ( -0.4800180268475474632, 0.1716606712744873642, 0.06108529706132549003 ) ) ;
#13792 = CARTESIAN_POINT ( 'NONE',  ( -5.731347020009612645E-17, 0.2263888888888885564, 0.3119999999999999996 ) ) ;
#13793 = CARTESIAN_POINT ( 'NONE',  ( 0.2819296736111110979, 4.231333333409199149, -0.1167790944451423396 ) ) ;
#13794 = CONTEXT_DEPENDENT_SHAPE_REPRESENTATION ( #9210, #1951 ) ;
#13795 = AXIS2_PLACEMENT_3D ( 'NONE', #1471, #6837, #5237 ) ;
#13796 = CARTESIAN_POINT ( 'NONE',  ( -0.0005878709530763284643, 4.043849134038319804, -0.3119994809580396988 ) ) ;
#13797 = CARTESIAN_POINT ( 'NONE',  ( 0.1144950937579611444, 0.2764156081756483641, 0.3001388888888924522 ) ) ;
#13798 = CARTESIAN_POINT ( 'NONE',  ( -0.1167790944451424368, 0.4208333332574665797, 0.2819296736111110424 ) ) ;
#13799 = CARTESIAN_POINT ( 'NONE',  ( 0.4000000000000000222, 0.4624999998049150740, 0.000000000000000000 ) ) ;
#13800 = CARTESIAN_POINT ( 'NONE',  ( 0.3119999999999999996, 4.467444444444443441, -3.820898013339742174E-17 ) ) ;
#13801 = LINE ( 'NONE', #21232, #13098 ) ;
#13802 = CARTESIAN_POINT ( 'NONE',  ( -0.3155070326520292845, 1.931923388228935888E-17, 0.1734027777777800983 ) ) ;
#13803 = CARTESIAN_POINT ( 'NONE',  ( 0.000000000000000000, 6.000000000000000888, 0.000000000000000000 ) ) ;
#13804 = CARTESIAN_POINT ( 'NONE',  ( -0.1167790944451422702, 0.5527777777019111660, -0.2819296736111110979 ) ) ;
#13805 = CARTESIAN_POINT ( 'NONE',  ( 0.1167790944451423535, 0.3027777777019111105, 0.2819296736111110424 ) ) ;
#13806 = CARTESIAN_POINT ( 'NONE',  ( 5.178964085587577574E-17, 3.991750000075865223, 0.2819296736111110979 ) ) ;
#13807 = CARTESIAN_POINT ( 'NONE',  ( 0.3236067977499790249, 0.3982142855192009057, -0.2351141009169892826 ) ) ;
#13808 = CARTESIAN_POINT ( 'NONE',  ( -0.2819296736111110979, 4.644527777853643791, 0.000000000000000000 ) ) ;
#13809 = EDGE_CURVE ( 'NONE', #795, #12482, #3523, .T. ) ;
#13810 = CARTESIAN_POINT ( 'NONE',  ( -0.2206173157302027954, 0.1430555554038226151, -0.2206173157302028232 ) ) ;
#13811 = ORIENTED_EDGE ( 'NONE', *, *, #15304, .T. ) ;
#13812 = EDGE_CURVE ( 'NONE', #12593, #11100, #17254, .T. ) ;
#13813 = ORIENTED_EDGE ( 'NONE', *, *, #22390, .T. ) ;
#13814 = CARTESIAN_POINT ( 'NONE',  ( -0.1294417382415922191, 0.3125000000000000000, 0.3904166666666711860 ) ) ;
#13815 = CARTESIAN_POINT ( 'NONE',  ( 0.3119999999999999996, 3.922305555707287006, -0.1292346314604056745 ) ) ;
#13816 = VECTOR ( 'NONE', #10519, 39.37007874015748143 ) ;
#13817 = LINE ( 'NONE', #17347, #16920 ) ;
#13818 = EDGE_CURVE ( 'NONE', #16523, #20947, #1350, .T. ) ;
#13819 = ORIENTED_EDGE ( 'NONE', *, *, #11988, .F. ) ;
#13820 = CIRCLE ( 'NONE', #16927, 0.2510000000000000009 ) ;
#13821 = APPLICATION_PROTOCOL_DEFINITION ( 'international standard', 'config_control_design', 1994, #22126 ) ;
#13822 = CARTESIAN_POINT ( 'NONE',  ( 0.2437787738197950693, 0.1452258864492554369, 0.3947958900003602500 ) ) ;
#13823 = CARTESIAN_POINT ( 'NONE',  ( -0.3115931849604412496, 5.001428069419088018, -0.02819374845571557750 ) ) ;
#13824 = ORIENTED_EDGE ( 'NONE', *, *, #5188, .F. ) ;
#13825 = CARTESIAN_POINT ( 'NONE',  ( -0.1167790944451424368, 0.03194444436857781650, 0.2819296736111110424 ) ) ;
#13826 = ORIENTED_EDGE ( 'NONE', *, *, #5352, .F. ) ;
#13827 = CARTESIAN_POINT ( 'NONE',  ( 0.04078511732514260996, 4.239493367616026909, 0.3120000055331293431 ) ) ;
#13828 = DIRECTION ( 'NONE',  ( 0.000000000000000000, 0.000000000000000000, 1.000000000000000000 ) ) ;
#13829 = DIRECTION ( 'NONE',  ( 1.000000000000000000, 0.000000000000000000, 0.000000000000000000 ) ) ;
#13830 = AXIS2_PLACEMENT_3D ( 'NONE', #19923, #9061, #17976 ) ;
#13831 = CARTESIAN_POINT ( 'NONE',  ( 2.326421213736078119E-17, 0.2258928570453146711, -0.3799334167787516425 ) ) ;
#13832 = CARTESIAN_POINT ( 'NONE',  ( 0.1784294693753899486, 5.172189122700864061, 0.2361384720919713631 ) ) ;
#13833 = CARTESIAN_POINT ( 'NONE',  ( -0.1116596296178199582, 0.2473214284738861346, -0.3436530038418508792 ) ) ;
#13834 = CARTESIAN_POINT ( 'NONE',  ( -0.3999999999999999667, 0.1374999998049151739, -0.1299678784931626030 ) ) ;
#13835 = CARTESIAN_POINT ( 'NONE',  ( -0.1993543840281266355, 5.207027777853642903, 0.1993543840281267465 ) ) ;
#13836 =( BOUNDED_CURVE ( )  B_SPLINE_CURVE ( 2, ( #4746, #1220, #6950, #12217, #6701, #6825, #21345, #8404, #8288 ),
 .UNSPECIFIED., .F., .F. ) 
 B_SPLINE_CURVE_WITH_KNOTS ( ( 3, 2, 2, 2, 3 ),
 ( 0.6041666666666667407, 0.6145833333333334814, 0.6250000000000000000, 0.6354166666666666297, 0.6458333333333333703 ),
 .UNSPECIFIED. ) 
 CURVE ( )  GEOMETRIC_REPRESENTATION_ITEM ( )  RATIONAL_B_SPLINE_CURVE ( ( 0.9999999999999992228, 0.9238795325112875156, 1.000000000000000000, 0.9238795325112867385, 1.000000000000000000, 0.9238795325112867385, 1.000000000000000000, 0.9238795325112867385, 1.000000000000000000 ) ) 
 REPRESENTATION_ITEM ( '' )  );
#13837 = CC_DESIGN_APPROVAL ( #4198, ( #6483 ) ) ;
#13838 =( BOUNDED_SURFACE ( )  B_SPLINE_SURFACE ( 1, 2, ( 
 ( #20159, #17397, #1740, #1857, #22338, #7590, #14919, #15042, #5641, #22464, #9300, #9058, #3691, #20757, #22221, #5764, #7470, #2101, #18568, #9181, #5520, #16624, #22102, #13224, #18685, #10898, #11378, #18328, #16975, #16862, #23, #14684, #1624, #20519, #20634, #12984, #3566, #3936, #23918, #12862, #24044, #13106, #20400, #11138, #14804, #3817, #147, #16741, #11259, #18444, #1987, #9423, #271, #5874, #18806, #5397, #9542, #20281, #7711, #15157, #22589, #11020, #7353, #13335, #16505, #7237, #15396, #508, #13458, #20876, #752, #4170, #13583, #10037, #15635, #20993, #9909, #17459, #15515, #2353, #11745, #4531, #8180, #2591, #11872, #19408, #22939, #10156, #634, #4288, #22823, #870, #18936, #17341, #2705, #17581, #11994, #23167, #19166, #21118, #9794, #2233, #6114, #17227, #2474, #7941, #8065, #22703, #8303, #15275, #23052, #11621, #19052, #6360, #6479, #6235, #4047, #4408, #13701, #15755, #13930, #19285, #13807, #21243, #11501, #9666, #17103, #391, #7830, #5993, #10274, #1237, #17699, #23409, #14162, #3178, #23285, #4885, #991, #2941, #15868 ),
 ( #8662, #8546, #15988, #1114, #14281, #10628, #12350, #6717, #4760, #6841, #21719, #10749, #16355, #19767, #8420, #19525, #6598, #3064, #21830, #16236, #18181, #21592, #19886, #14046, #10511, #2818, #17941, #21477, #1353, #16111, #5003, #7087, #23524, #12464, #23646, #12232, #18057, #8784, #6966, #14406, #5121, #19642, #12586, #10399, #17822, #20009, #3295, #1474, #8912, #23766, #21361, #4648, #12115, #10992, #7204, #3659, #18536, #9394, #7559, #24015, #10870, #5242, #18299, #16593, #20487, #22309, #16834, #18417, #9271, #9032, #7325, #12714, #1711, #20128, #7443, #9150, #1826, #22432, #14777, #20368, #5607, #23886, #20251, #22191, #5490, #14527, #1597, #12956, #23593, #14650, #11106, #15012, #117, #16712, #14890, #5367, #13072, #3539, #3420, #16475, #3783, #11227, #18656, #1948, #21949, #22071, #12833, #23600, #1432, #14232, #19962, #18134, #7041, #23716, #4833, #1187, #23478, #3374, #10698, #6915, #7161, #12301, #14602, #10825, #5194, #3133, #2885, #8985, #6669, #6793, #23839, #14480, #15935, #14354, #3250, #3018, #10585, #21786, #8859, #16188, #16303 ) ),
 .UNSPECIFIED., .F., .F., .F. ) 
 B_SPLINE_SURFACE_WITH_KNOTS ( ( 2, 2 ),
 ( 3, 2, 2, 2, 2, 2, 2, 2, 2, 2, 2, 2, 2, 2, 2, 2, 2, 2, 2, 2, 2, 2, 2, 2, 2, 2, 2, 2, 2, 2, 2, 2, 2, 2, 2, 2, 2, 2, 2, 2, 2, 2, 2, 2, 2, 2, 2, 2, 2, 2, 2, 2, 2, 2, 2, 2, 2, 2, 2, 2, 2, 2, 2, 2, 2, 2, 2, 2, 2, 2, 3 ),
 ( 0.000000000000000000, 1.000000000000000000 ),
 ( 0.000000000000000000, 0.01428571428571428527, 0.02857142857142857054, 0.04285714285714285754, 0.05714285714285714107, 0.07142857142857142461, 0.08571428571428571508, 0.1000000000000000056, 0.1142857142857142821, 0.1285714285714285587, 0.1428571428571428492, 0.1571428571428571397, 0.1714285714285714302, 0.1857142857142857206, 0.2000000000000000111, 0.2142857142857142738, 0.2285714285714285643, 0.2428571428571428548, 0.2571428571428571175, 0.2714285714285714080, 0.2857142857142856984, 0.2999999999999999889, 0.3142857142857142794, 0.3285714285714285698, 0.3428571428571428603, 0.3571428571428571508, 0.3714285714285714413, 0.3857142857142857317, 0.4000000000000000222, 0.4142857142857143127, 0.4285714285714285476, 0.4428571428571428381, 0.4571428571428571286, 0.4714285714285714191, 0.4857142857142857095, 0.5000000000000000000, 0.5142857142857142350, 0.5285714285714285809, 0.5428571428571428159, 0.5571428571428571619, 0.5714285714285713969, 0.5857142857142857428, 0.5999999999999999778, 0.6142857142857143238, 0.6285714285714285587, 0.6428571428571429047, 0.6571428571428571397, 0.6714285714285713746, 0.6857142857142857206, 0.6999999999999999556, 0.7142857142857143016, 0.7285714285714285365, 0.7428571428571428825, 0.7571428571428571175, 0.7714285714285714635, 0.7857142857142856984, 0.8000000000000000444, 0.8142857142857142794, 0.8285714285714286254, 0.8428571428571428603, 0.8571428571428570953, 0.8714285714285714413, 0.8857142857142856762, 0.9000000000000000222, 0.9142857142857142572, 0.9285714285714286031, 0.9428571428571428381, 0.9571428571428571841, 0.9714285714285714191, 0.9857142857142857650, 1.000000000000000000 ),
 .UNSPECIFIED. ) 
 GEOMETRIC_REPRESENTATION_ITEM ( )  RATIONAL_B_SPLINE_SURFACE ( (
 ( 1.000000000000000000, 0.9510565162951535312, 1.000000000000000000, 0.9510565162951535312, 1.000000000000000000, 0.9510565162951535312, 1.000000000000000000, 0.9510565162951535312, 1.000000000000000000, 0.9510565162951535312, 1.000000000000000000, 0.9510565162951535312, 1.000000000000000000, 0.9510565162951535312, 1.000000000000000000, 0.9510565162951535312, 1.000000000000000000, 0.9510565162951535312, 1.000000000000000000, 0.9510565162951535312, 1.000000000000000000, 0.9510565162951535312, 1.000000000000000000, 0.9510565162951535312, 1.000000000000000000, 0.9510565162951535312, 1.000000000000000000, 0.9510565162951535312, 1.000000000000000000, 0.9510565162951535312, 1.000000000000000000, 0.9510565162951535312, 1.000000000000000000, 0.9510565162951535312, 1.000000000000000000, 0.9510565162951535312, 1.000000000000000000, 0.9510565162951535312, 1.000000000000000000, 0.9510565162951535312, 1.000000000000000000, 0.9510565162951535312, 1.000000000000000000, 0.9510565162951535312, 1.000000000000000000, 0.9510565162951535312, 1.000000000000000000, 0.9510565162951535312, 1.000000000000000000, 0.9510565162951535312, 1.000000000000000000, 0.9510565162951535312, 1.000000000000000000, 0.9510565162951535312, 1.000000000000000000, 0.9510565162951535312, 1.000000000000000000, 0.9510565162951535312, 1.000000000000000000, 0.9510565162951535312, 1.000000000000000000, 0.9510565162951535312, 1.000000000000000000, 0.9510565162951535312, 1.000000000000000000, 0.9510565162951535312, 1.000000000000000000, 0.9510565162951535312, 1.000000000000000000, 0.9510565162951535312, 1.000000000000000000, 0.9510565162951535312, 1.000000000000000000, 0.9510565162951535312, 1.000000000000000000, 0.9510565162951535312, 1.000000000000000000, 0.9510565162951535312, 1.000000000000000000, 0.9510565162951535312, 1.000000000000000000, 0.9510565162951535312, 1.000000000000000000, 0.9510565162951535312, 1.000000000000000000, 0.9510565162951535312, 1.000000000000000000, 0.9510565162951535312, 1.000000000000000000, 0.9510565162951535312, 1.000000000000000000, 0.9510565162951535312, 1.000000000000000000, 0.9510565162951535312, 1.000000000000000000, 0.9510565162951535312, 1.000000000000000000, 0.9510565162951535312, 1.000000000000000000, 0.9510565162951535312, 1.000000000000000000, 0.9510565162951535312, 1.000000000000000000, 0.9510565162951535312, 1.000000000000000000, 0.9510565162951535312, 1.000000000000000000, 0.9510565162951535312, 1.000000000000000000, 0.9510565162951535312, 1.000000000000000000, 0.9510565162951535312, 1.000000000000000000, 0.9510565162951535312, 1.000000000000000000, 0.9510565162951535312, 1.000000000000000000, 0.9510565162951535312, 1.000000000000000000, 0.9510565162951535312, 1.000000000000000000, 0.9510565162951535312, 1.000000000000000000, 0.9510565162951535312, 1.000000000000000000, 0.9510565162951535312, 1.000000000000000000, 0.9510565162951535312, 1.000000000000000000, 0.9510565162951535312, 1.000000000000000000, 0.9510565162951535312, 1.000000000000000000, 0.9510565162951535312, 1.000000000000000000, 0.9510565162951535312, 1.000000000000000000, 0.9510565162951535312, 1.000000000000000000, 0.9510565162951535312, 1.000000000000000000),
 ( 1.000000000000000000, 0.9510565162951535312, 1.000000000000000000, 0.9510565162951535312, 1.000000000000000000, 0.9510565162951535312, 1.000000000000000000, 0.9510565162951535312, 1.000000000000000000, 0.9510565162951535312, 1.000000000000000000, 0.9510565162951535312, 1.000000000000000000, 0.9510565162951535312, 1.000000000000000000, 0.9510565162951535312, 1.000000000000000000, 0.9510565162951535312, 1.000000000000000000, 0.9510565162951535312, 1.000000000000000000, 0.9510565162951535312, 1.000000000000000000, 0.9510565162951535312, 1.000000000000000000, 0.9510565162951535312, 1.000000000000000000, 0.9510565162951535312, 1.000000000000000000, 0.9510565162951535312, 1.000000000000000000, 0.9510565162951535312, 1.000000000000000000, 0.9510565162951535312, 1.000000000000000000, 0.9510565162951535312, 1.000000000000000000, 0.9510565162951535312, 1.000000000000000000, 0.9510565162951535312, 1.000000000000000000, 0.9510565162951535312, 1.000000000000000000, 0.9510565162951535312, 1.000000000000000000, 0.9510565162951535312, 1.000000000000000000, 0.9510565162951535312, 1.000000000000000000, 0.9510565162951535312, 1.000000000000000000, 0.9510565162951535312, 1.000000000000000000, 0.9510565162951535312, 1.000000000000000000, 0.9510565162951535312, 1.000000000000000000, 0.9510565162951535312, 1.000000000000000000, 0.9510565162951535312, 1.000000000000000000, 0.9510565162951535312, 1.000000000000000000, 0.9510565162951535312, 1.000000000000000000, 0.9510565162951535312, 1.000000000000000000, 0.9510565162951535312, 1.000000000000000000, 0.9510565162951535312, 1.000000000000000000, 0.9510565162951535312, 1.000000000000000000, 0.9510565162951535312, 1.000000000000000000, 0.9510565162951535312, 1.000000000000000000, 0.9510565162951535312, 1.000000000000000000, 0.9510565162951535312, 1.000000000000000000, 0.9510565162951535312, 1.000000000000000000, 0.9510565162951535312, 1.000000000000000000, 0.9510565162951535312, 1.000000000000000000, 0.9510565162951535312, 1.000000000000000000, 0.9510565162951535312, 1.000000000000000000, 0.9510565162951535312, 1.000000000000000000, 0.9510565162951535312, 1.000000000000000000, 0.9510565162951535312, 1.000000000000000000, 0.9510565162951535312, 1.000000000000000000, 0.9510565162951535312, 1.000000000000000000, 0.9510565162951535312, 1.000000000000000000, 0.9510565162951535312, 1.000000000000000000, 0.9510565162951535312, 1.000000000000000000, 0.9510565162951535312, 1.000000000000000000, 0.9510565162951535312, 1.000000000000000000, 0.9510565162951535312, 1.000000000000000000, 0.9510565162951535312, 1.000000000000000000, 0.9510565162951535312, 1.000000000000000000, 0.9510565162951535312, 1.000000000000000000, 0.9510565162951535312, 1.000000000000000000, 0.9510565162951535312, 1.000000000000000000, 0.9510565162951535312, 1.000000000000000000, 0.9510565162951535312, 1.000000000000000000, 0.9510565162951535312, 1.000000000000000000, 0.9510565162951535312, 1.000000000000000000, 0.9510565162951535312, 1.000000000000000000, 0.9510565162951535312, 1.000000000000000000, 0.9510565162951535312, 1.000000000000000000, 0.9510565162951535312, 1.000000000000000000, 0.9510565162951535312, 1.000000000000000000) ) ) 
 REPRESENTATION_ITEM ( '' )  SURFACE ( )  );
#13839 = CARTESIAN_POINT ( 'NONE',  ( 0.5097595264191659981, 2.291712385858714729, -0.6667552972947653478 ) ) ;
#13840 = AXIS2_PLACEMENT_3D ( 'NONE', #1836, #5501, #20857 ) ;
#13841 = CARTESIAN_POINT ( 'NONE',  ( 5.253288188650943643E-17, 5.197747365142496356, 0.2859756893339090444 ) ) ;
#13842 = CARTESIAN_POINT ( 'NONE',  ( 0.2206173157302028232, 0.3513888887371559577, -0.2206173157302028232 ) ) ;
#13843 = CARTESIAN_POINT ( 'NONE',  ( -0.3119999999999999996, 4.498694444596177178, -0.1292346314604056468 ) ) ;
#13844 = CARTESIAN_POINT ( 'NONE',  ( -0.2819296736111110979, 4.977861111186976828, 0.000000000000000000 ) ) ;
#13845 = VERTEX_POINT ( 'NONE', #23643 ) ;
#13846 = CARTESIAN_POINT ( 'NONE',  ( -1.726321361862525858E-17, 4.172305555631420582, -0.2819296736111110979 ) ) ;
#13847 = CARTESIAN_POINT ( 'NONE',  ( 0.3613381517857143232, 0.2830357141881718053, -0.1174058825155740587 ) ) ;
#13848 = VECTOR ( 'NONE', #16337, 39.37007874015748854 ) ;
#13849 = EDGE_CURVE ( 'NONE', #21597, #5324, #17819, .T. ) ;
#13850 = ORIENTED_EDGE ( 'NONE', *, *, #11865, .T. ) ;
#13851 = CALENDAR_DATE ( 2026, 7, 10 ) ;
#13852 = CARTESIAN_POINT ( 'NONE',  ( -0.1916493530484528196, -0.4197546306156789697, 0.4334994210334168208 ) ) ;
#13853 = FACE_OUTER_BOUND ( 'NONE', #21732, .T. ) ;
#13854 = SECURITY_CLASSIFICATION ( '', '', #14454 ) ;
#13855 = ORIENTED_EDGE ( 'NONE', *, *, #8117, .T. ) ;
#13856 = FACE_OUTER_BOUND ( 'NONE', #10844, .T. ) ;
#13857 = CARTESIAN_POINT ( 'NONE',  ( -0.2195630361087207438, -0.1679215936615484350, -0.06558227484231504700 ) ) ;
#13858 = CARTESIAN_POINT ( 'NONE',  ( 0.1988757138996042617, 3.752970977545328157, -0.2404006040361021113 ) ) ;
#13859 = CARTESIAN_POINT ( 'NONE',  ( -0.3125000000000000555, 1.913510623667739771E-17, 0.2897222222222258226 ) ) ;
#13860 = VERTEX_POINT ( 'NONE', #17696 ) ;
#13861 = DIRECTION ( 'NONE',  ( -0.000000000000000000, -0.000000000000000000, -1.000000000000000000 ) ) ;
#13862 = CARTESIAN_POINT ( 'NONE',  ( 0.2658661084243346684, 0.03242967361111057795, 0.09380593400082704036 ) ) ;
#13863 = CARTESIAN_POINT ( 'NONE',  ( -0.1144950937579609779, 0.2764156081756484196, 0.07791666666666847985 ) ) ;
#13864 = ORIENTED_EDGE ( 'NONE', *, *, #13409, .T. ) ;
#13865 = CYLINDRICAL_SURFACE ( 'NONE', #7758, 0.4000000000000000222 ) ;
#13866 = AXIS2_PLACEMENT_3D ( 'NONE', #5053, #8963, #1530 ) ;
#13867 = CARTESIAN_POINT ( 'NONE',  ( 0.2819296736111110424, 4.606333333409200037, -0.1167790944451423396 ) ) ;
#13868 = CARTESIAN_POINT ( 'NONE',  ( -0.2802773643484119392, 0.009513829220699217271, -0.06944403101507866383 ) ) ;
#13869 = CARTESIAN_POINT ( 'NONE',  ( -0.2869978706053274431, 0.3497335006013223002, -1.162630022054959467 ) ) ;
#13870 = DIRECTION ( 'NONE',  ( -0.6374213576849414586, 0.000000000000000000, 0.7705154202007158393 ) ) ;
#13871 = SPHERICAL_SURFACE ( 'NONE', #19747, 0.01874999999999999931 ) ;
#13872 = CARTESIAN_POINT ( 'NONE',  ( 0.2206173157302028787, 4.293833333333332725, 0.2206173157302027954 ) ) ;
#13873 = CARTESIAN_POINT ( 'NONE',  ( -0.3119999999999999996, 5.168833333485065573, 0.000000000000000000 ) ) ;
#13874 = CARTESIAN_POINT ( 'NONE',  ( -5.488040394358968970E-07, 4.960478275469978549, 0.3119999999989728212 ) ) ;
#13875 = CC_DESIGN_DATE_AND_TIME_ASSIGNMENT ( #18342, #7252, ( #13174 ) ) ;
#13876 = CARTESIAN_POINT ( 'NONE',  ( 0.3950000000000000178, 2.978485840173427324, -0.2605837454876624437 ) ) ;
#13877 = EDGE_LOOP ( 'NONE', ( #11184, #7143, #17492, #12561 ) ) ;
#13878 = DIRECTION ( 'NONE',  ( -1.177540334020096294E-17, 0.2588190451025213501, -0.9659258262890680902 ) ) ;
#13879 = VERTEX_POINT ( 'NONE', #3292 ) ;
#13880 = CARTESIAN_POINT ( 'NONE',  ( 0.05352797175791356582, 4.684214349109525166, 0.3073846428649295581 ) ) ;
#13881 = VECTOR ( 'NONE', #5857, 39.37007874015748854 ) ;
#13882 = UNCERTAINTY_MEASURE_WITH_UNIT (LENGTH_MEASURE( 1.000000000000000082E-05 ), #12842, 'distance_accuracy_value', 'NONE');
#13883 = CARTESIAN_POINT ( 'NONE',  ( 0.1909493018183467117, 4.133023247099400166, 0.2467435441855950762 ) ) ;
#13884 = CARTESIAN_POINT ( 'NONE',  ( 0.1306872919485616846, 0.3155070326520292290, -0.06270833333333244997 ) ) ;
#13885 = CARTESIAN_POINT ( 'NONE',  ( -0.009374999999999905978, -0.5358532185916218271, 0.06112444011295371793 ) ) ;
#13886 = ORIENTED_EDGE ( 'NONE', *, *, #12510, .T. ) ;
#13887 = CARTESIAN_POINT ( 'NONE',  ( -0.3613381517857143232, 0.02589285704531474330, -0.1174058825155741004 ) ) ;
#13888 = CARTESIAN_POINT ( 'NONE',  ( 0.2819296736111110979, 0.04930555547968892144, 0.000000000000000000 ) ) ;
#13889 = CARTESIAN_POINT ( 'NONE',  ( -0.2764156081756484196, 0.1144950937579609918, 0.09180555555555744429 ) ) ;
#13890 = CARTESIAN_POINT ( 'NONE',  ( -0.5116234456863258950, 1.999640111863030256, -2.727383698113316157 ) ) ;
#13891 = PLANE ( 'NONE',  #17947 ) ;
#13892 = CYLINDRICAL_SURFACE ( 'NONE', #14375, 0.3119999999999999996 ) ;
#13893 = ORIENTED_EDGE ( 'NONE', *, *, #5457, .F. ) ;
#13894 = DIRECTION ( 'NONE',  ( -0.8660254037844434816, -0.000000000000000000, 0.4999999999999914513 ) ) ;
#13895 = CARTESIAN_POINT ( 'NONE',  ( -0.3129426082665457964, 4.280301605886003280, 0.01319854631990339047 ) ) ;
#13896 = CARTESIAN_POINT ( 'NONE',  ( 0.000000000000000000, 5.384999999999999787, 0.000000000000000000 ) ) ;
#13897 = CARTESIAN_POINT ( 'NONE',  ( 0.2206173157302027676, 0.5111111111111107386, 0.2206173157302028787 ) ) ;
#13898 = CARTESIAN_POINT ( 'NONE',  ( -0.1292346314604056745, 4.929249999999999687, -0.3119999999999999996 ) ) ;
#13899 = CC_DESIGN_PERSON_AND_ORGANIZATION_ASSIGNMENT ( #21254, #6732, ( #8009 ) ) ;
#13900 = CARTESIAN_POINT ( 'NONE',  ( -0.1167790944451423257, 3.967444444520310309, -0.2819296736111110424 ) ) ;
#13901 = DIRECTION ( 'NONE',  ( 0.4999999999999912292, 0.000000000000000000, -0.8660254037844437036 ) ) ;
#13902 = CARTESIAN_POINT ( 'NONE',  ( 1.779986855112097865, 2.978485840173427324, -2.386288568296997870 ) ) ;
#13903 = DIRECTION ( 'NONE',  ( 0.000000000000000000, 0.000000000000000000, 1.000000000000000000 ) ) ;
#13904 = ORIENTED_EDGE ( 'NONE', *, *, #19300, .F. ) ;
#13905 = ORIENTED_EDGE ( 'NONE', *, *, #13192, .T. ) ;
#13906 = CARTESIAN_POINT ( 'NONE',  ( 0.3125000000000009437, 0.1294417382415912476, 0.09875000000000208611 ) ) ;
#13907 = CARTESIAN_POINT ( 'NONE',  ( -0.2819296736111110979, 4.630638888964754507, 0.000000000000000000 ) ) ;
#13908 = CARTESIAN_POINT ( 'NONE',  ( -0.2923287055106771337, 0.3937499999024575148, 0.2123892367102619971 ) ) ;
#13909 = LINE ( 'NONE', #22801, #4470 ) ;
#13910 = APPROVAL_ROLE ( '' ) ;
#13911 = CARTESIAN_POINT ( 'NONE',  ( 0.4700000000000002509, 2.740000000000000213, -0.6252851813312900742 ) ) ;
#13912 = CARTESIAN_POINT ( 'NONE',  ( -0.2764156081756484196, 0.1144950937579609918, -0.08180555555555503455 ) ) ;
#13913 = AXIS2_PLACEMENT_3D ( 'NONE', #3558, #9170, #16615 ) ;
#13914 = CARTESIAN_POINT ( 'NONE',  ( -1.726321361862525858E-17, 4.019527777853643791, -0.2819296736111110979 ) ) ;
#13915 = SECURITY_CLASSIFICATION_LEVEL ( 'unclassified' ) ;
#13916 = CARTESIAN_POINT ( 'NONE',  ( -0.1877440169500084466, 4.827352557465903082, -0.2523603461020555438 ) ) ;
#13917 = CARTESIAN_POINT ( 'NONE',  ( -0.3308333333333332571, 4.088927411497558688E-17, 0.4425000000000000044 ) ) ;
#13918 = CARTESIAN_POINT ( 'NONE',  ( -0.2764156081756484196, 1.692557448933383907E-17, 0.3175000000000036682 ) ) ;
#13919 = CARTESIAN_POINT ( 'NONE',  ( -0.1294417382415922746, -0.3125000000000000000, 0.3556944444444486986 ) ) ;
#13920 = CARTESIAN_POINT ( 'NONE',  ( -0.2819296736111110979, 0.007638888813022256218, -3.452642723725051716E-17 ) ) ;
#13921 = CARTESIAN_POINT ( 'NONE',  ( 1.910449006669871087E-17, 0.4208333333333330040, -0.3119999999999999996 ) ) ;
#13922 = CARTESIAN_POINT ( 'NONE',  ( -0.08367472778091829266, 0.4929562507565926621, 0.07813238993955247402 ) ) ;
#13923 = CARTESIAN_POINT ( 'NONE',  ( -0.2472135954999579999, 0.3749999999999999445, 0.3402603233408159622 ) ) ;
#13924 = CARTESIAN_POINT ( 'NONE',  ( -0.2230971623002954152, -0.2230971623002953874, 0.4025694444444485876 ) ) ;
#13925 = EDGE_LOOP ( 'NONE', ( #16040, #2607, #821, #11732 ) ) ;
#13926 = CARTESIAN_POINT ( 'NONE',  ( -0.4593750000000004219, -0.2760455974562901482, 0.3779506566538942125 ) ) ;
#13927 = CARTESIAN_POINT ( 'NONE',  ( 0.2819296736111110979, 0.4277777777019111660, -0.1167790944451422980 ) ) ;
#13928 = CARTESIAN_POINT ( 'NONE',  ( 0.1167790944451423535, 0.5249999999241333759, 0.2819296736111110424 ) ) ;
#13929 = CARTESIAN_POINT ( 'NONE',  ( 0.2819296736111110979, 4.116750000075866112, -3.452642723725051716E-17 ) ) ;
#13930 = CARTESIAN_POINT ( 'NONE',  ( 0.4000000000000000222, 0.3910714283763437327, 0.000000000000000000 ) ) ;
#13931 = EDGE_CURVE ( 'NONE', #19658, #3680, #18028, .T. ) ;
#13932 = CARTESIAN_POINT ( 'NONE',  ( -0.2819296736111110424, 4.752166666742533074, -0.1167790944451423119 ) ) ;
#13933 = DIRECTION ( 'NONE',  ( -0.4985709748471494063, -0.07555085810113112976, 0.8635502596144279952 ) ) ;
#13934 = DIRECTION ( 'NONE',  ( -1.000000000000000000, 0.000000000000000000, 0.000000000000000000 ) ) ;
#13935 = ORIENTED_EDGE ( 'NONE', *, *, #8548, .F. ) ;
#13936 = CIRCLE ( 'NONE', #15472, 0.1874999999999998335 ) ;
#13937 = DIRECTION ( 'NONE',  ( 1.707404996040164512E-16, 0.000000000000000000, -1.000000000000000000 ) ) ;
#13938 = CARTESIAN_POINT ( 'NONE',  ( 0.1292346314604056190, 3.818138889040621375, -0.3119999999999999996 ) ) ;
#13939 = DIRECTION ( 'NONE',  ( 0.000000000000000000, 0.000000000000000000, -1.000000000000000000 ) ) ;
#13940 = ORIENTED_EDGE ( 'NONE', *, *, #13051, .F. ) ;
#13941 = CARTESIAN_POINT ( 'NONE',  ( 0.06864889549624120235, 5.206640035683666845, 0.2739922474530114282 ) ) ;
#13942 = PERSON_AND_ORGANIZATION ( #15518, #2538 ) ;
#13943 = VERTEX_POINT ( 'NONE', #8781 ) ;
#13944 = PLANE ( 'NONE',  #5792 ) ;
#13945 = ORIENTED_EDGE ( 'NONE', *, *, #4146, .F. ) ;
#13946 = CARTESIAN_POINT ( 'NONE',  ( -0.1993543840281267465, 0.1395833332574666907, 0.1993543840281266633 ) ) ;
#13947 = EDGE_CURVE ( 'NONE', #14330, #9147, #23406, .T. ) ;
#13948 = AXIS2_PLACEMENT_3D ( 'NONE', #11712, #11594, #2675 ) ;
#13949 = ORIENTED_EDGE ( 'NONE', *, *, #2887, .F. ) ;
#13950 = CARTESIAN_POINT ( 'NONE',  ( 0.3037827064340575256, 4.249802897613654373, 0.08205749792799824083 ) ) ;
#13951 = CARTESIAN_POINT ( 'NONE',  ( -4.974594353761572974E-07, 4.738258141874186258, 0.3119999999991586170 ) ) ;
#13952 = CARTESIAN_POINT ( 'NONE',  ( 0.3016382822107275818, 4.083242817246184764, 0.07973931868136807655 ) ) ;
#13953 = CARTESIAN_POINT ( 'NONE',  ( 0.3613381517857143232, 0.2044642856167432632, 0.1174058825155742114 ) ) ;
#13954 = CARTESIAN_POINT ( 'NONE',  ( -0.2296906778660977588, 5.064311450068244014, 0.2111546458865629639 ) ) ;
#13955 = CARTESIAN_POINT ( 'NONE',  ( -0.4687500000000003886, -0.2598076211353319009, 0.4425000000000000044 ) ) ;
#13956 = DIRECTION ( 'NONE',  ( -0.000000000000000000, -1.000000000000000000, -0.000000000000000000 ) ) ;
#13957 = EDGE_CURVE ( 'NONE', #21366, #9589, #3084, .T. ) ;
#13958 = CARTESIAN_POINT ( 'NONE',  ( 0.1167790944451424368, 5.217444444520309865, 0.2819296736111110424 ) ) ;
#13959 = CARTESIAN_POINT ( 'NONE',  ( 0.2373038722028483205, 5.036289568926800797, -0.2041309936366799416 ) ) ;
#13960 = DIRECTION ( 'NONE',  ( -1.000000000000000000, 0.000000000000000000, -0.000000000000000000 ) ) ;
#13961 = CARTESIAN_POINT ( 'NONE',  ( -0.2802017012671415008, 4.784146520345384346, 0.1428922795062084750 ) ) ;
#13962 = CARTESIAN_POINT ( 'NONE',  ( 0.3119999999999999996, 4.582027777929510215, 0.1292346314604056190 ) ) ;
#13963 = CARTESIAN_POINT ( 'NONE',  ( 0.2819296736111110979, 4.620222222298088433, -0.1167790944451423396 ) ) ;
#13964 = VERTEX_POINT ( 'NONE', #21474 ) ;
#13965 = CARTESIAN_POINT ( 'NONE',  ( 0.1993543840281266633, 4.109805555631420582, -0.1993543840281266910 ) ) ;
#13966 = VECTOR ( 'NONE', #19936, 39.37007874015748854 ) ;
#13967 = VERTEX_POINT ( 'NONE', #23521 ) ;
#13968 = APPROVAL_DATE_TIME ( #8339, #1200 ) ;
#13969 = VERTEX_POINT ( 'NONE', #12229 ) ;
#13970 = CARTESIAN_POINT ( 'NONE',  ( 0.4336681474472749986, 3.704141657475161331, -2.371204961265731104 ) ) ;
#13971 = CYLINDRICAL_SURFACE ( 'NONE', #22135, 0.3119999999999999996 ) ;
#13972 = CARTESIAN_POINT ( 'NONE',  ( -0.1167790944451423119, 3.745222222298088433, -0.2819296736111110979 ) ) ;
#13973 = CARTESIAN_POINT ( 'NONE',  ( 0.7108475124358382136, 4.111524471938507119, -3.019372695974962717 ) ) ;
#13974 = CARTESIAN_POINT ( 'NONE',  ( -0.4592086519660381616, -0.09034263136374838521, 0.4297010434978499327 ) ) ;
#13975 = LINE ( 'NONE', #11919, #19417 ) ;
#13976 =( BOUNDED_SURFACE ( )  B_SPLINE_SURFACE ( 3, 2, ( 
 ( #8107, #6045, #20687 ),
 ( #9595, #2282, #2637 ),
 ( #15204, #9841, #4336 ),
 ( #20926, #2402, #11787 ),
 ( #19212, #19096, #17391 ),
 ( #3979, #7874, #15090 ),
 ( #4456, #4219, #11430 ),
 ( #13384, #17153, #20807 ),
 ( #684, #15562, #22513 ),
 ( #17273, #11673, #22984 ) ),
 .UNSPECIFIED., .F., .F., .T. ) 
 B_SPLINE_SURFACE_WITH_KNOTS ( ( 4, 2, 2, 2, 4 ),
 ( 3, 3 ),
 ( 0.04463809143445898742, 0.04796255359614957914, 0.05128701575784017086, 0.05461147791953076258, 0.05793594008122136124 ),
 ( 0.000000000000000000, 1.000000000000000000 ),
 .UNSPECIFIED. ) 
 GEOMETRIC_REPRESENTATION_ITEM ( )  RATIONAL_B_SPLINE_SURFACE ( (
 ( 1.000000000000000000, 0.8285407536241361504, 1.000000000000000000),
 ( 1.000000000000000000, 0.8326168960428316224, 1.000000000000000000),
 ( 1.000000000000000000, 0.8363786027323955041, 1.000000000000000000),
 ( 1.000000000000000000, 0.8417912930207277489, 1.000000000000000000),
 ( 1.000000000000000000, 0.8433923807913777937, 1.000000000000000000),
 ( 1.000000000000000000, 0.8433905099820321327, 1.000000000000000000),
 ( 1.000000000000000000, 0.8417888685867314091, 1.000000000000000000),
 ( 1.000000000000000000, 0.8363766775004335408, 1.000000000000000000),
 ( 1.000000000000000000, 0.8326159398059326255, 1.000000000000000000),
 ( 1.000000000000000000, 0.8285407536241353732, 1.000000000000000000) ) ) 
 REPRESENTATION_ITEM ( '' )  SURFACE ( )  );
#13977 =( BOUNDED_CURVE ( )  B_SPLINE_CURVE ( 2, ( #12795, #1915, #13037 ),
 .UNSPECIFIED., .F., .F. ) 
 B_SPLINE_CURVE_WITH_KNOTS ( ( 3, 3 ),
 ( 0.09727559839650132267, 0.09732137976955804182 ),
 .UNSPECIFIED. ) 
 CURVE ( )  GEOMETRIC_REPRESENTATION_ITEM ( )  RATIONAL_B_SPLINE_CURVE ( ( 0.9747197555285191939, 0.9751720984492913136, 0.9756404518778661883 ) ) 
 REPRESENTATION_ITEM ( '' )  );
#13978 = AXIS2_PLACEMENT_3D ( 'NONE', #18315, #7104, #3676 ) ;
#13979 = ORIENTED_EDGE ( 'NONE', *, *, #17650, .T. ) ;
#13980 = DIRECTION ( 'NONE',  ( -0.000000000000000000, -1.000000000000000000, -0.000000000000000000 ) ) ;
#13981 = CARTESIAN_POINT ( 'NONE',  ( 0.1167790944451423535, 0.1361111110352444808, 0.2819296736111110979 ) ) ;
#13982 = CARTESIAN_POINT ( 'NONE',  ( -0.2764156081756484196, 1.692557448933383907E-17, -0.02277777777777679341 ) ) ;
#13983 = LINE ( 'NONE', #6412, #3864 ) ;
#13984 = EDGE_CURVE ( 'NONE', #13733, #20678, #15865, .T. ) ;
#13985 = CARTESIAN_POINT ( 'NONE',  ( 0.2819296736111110424, 4.495222222298087544, -0.1167790944451423396 ) ) ;
#13986 = CARTESIAN_POINT ( 'NONE',  ( 5.178964085587577574E-17, 5.200083333409199149, 0.2819296736111110979 ) ) ;
#13987 = CARTESIAN_POINT ( 'NONE',  ( -0.1114086484834320989, 0.7676189894794268609, -1.079857323803883107 ) ) ;
#13988 = CARTESIAN_POINT ( 'NONE',  ( -0.1294417382415922746, -0.3125000000000000000, -0.04013888888888822448 ) ) ;
#13989 = CARTESIAN_POINT ( 'NONE',  ( 0.3119999999999999996, 4.248694444444443441, -0.1292346314604056745 ) ) ;
#13990 = CARTESIAN_POINT ( 'NONE',  ( 0.2206173157302028787, 5.189666666818398610, 0.2206173157302027954 ) ) ;
#13991 = CARTESIAN_POINT ( 'NONE',  ( 0.000000000000000000, 2.735000000000000320, 0.000000000000000000 ) ) ;
#13992 = DIRECTION ( 'NONE',  ( 0.000000000000000000, 0.000000000000000000, -1.000000000000000000 ) ) ;
#13993 = EDGE_LOOP ( 'NONE', ( #19084, #22453, #16034, #16558 ) ) ;
#13994 = CARTESIAN_POINT ( 'NONE',  ( -0.1275151006136568121, 4.880904689916613748, -0.2851559274793544763 ) ) ;
#13995 = AXIS2_PLACEMENT_3D ( 'NONE', #15918, #8476, #8939 ) ;
#13996 = CARTESIAN_POINT ( 'NONE',  ( 0.4687500000000003886, -0.2598076211353317344, 0.06112444011295375262 ) ) ;
#13997 = CARTESIAN_POINT ( 'NONE',  ( 0.3155070326520292845, -5.795770164686806123E-17, 0.09354166666666878516 ) ) ;
#13998 = CARTESIAN_POINT ( 'NONE',  ( 0.2022257292156428021, 0.4370114112024169328, 0.07440066028686925792 ) ) ;
#13999 = DIRECTION ( 'NONE',  ( 0.000000000000000000, 1.000000000000000000, 0.000000000000000000 ) ) ;
#14000 = CARTESIAN_POINT ( 'NONE',  ( -0.1116596296178199582, 0.3008928570453147100, -0.3436530038418508792 ) ) ;
#14001 = CARTESIAN_POINT ( 'NONE',  ( -5.178964085587577574E-17, 0.09097222214635558579, 0.2819296736111110979 ) ) ;
#14002 = CARTESIAN_POINT ( 'NONE',  ( -0.1954553509668046640, 0.1954553509668046918, -0.07833333333333279691 ) ) ;
#14003 = CARTESIAN_POINT ( 'NONE',  ( -0.3125000000000000000, 1.913510623667739771E-17, -0.04361111111111011518 ) ) ;
#14004 = CARTESIAN_POINT ( 'NONE',  ( -3.827021247335479543E-17, -0.3125000000000000000, 0.07444444444444603404 ) ) ;
#14005 = CARTESIAN_POINT ( 'NONE',  ( -0.1144950937579609779, 0.2764156081756484196, 0.4737500000000048894 ) ) ;
#14006 = ORIENTED_EDGE ( 'NONE', *, *, #23418, .F. ) ;
#14007 = EDGE_CURVE ( 'NONE', #17359, #7539, #19087, .T. ) ;
#14008 = CARTESIAN_POINT ( 'NONE',  ( 0.000000000000000000, 0.9300000000000000488, 0.000000000000000000 ) ) ;
#14009 = CARTESIAN_POINT ( 'NONE',  ( -0.001077020842221716127, 4.293802776323909498, 0.3119984097836999148 ) ) ;
#14010 = DIRECTION ( 'NONE',  ( 0.000000000000000000, 0.000000000000000000, -1.000000000000000000 ) ) ;
#14011 = CARTESIAN_POINT ( 'NONE',  ( 0.2206173157302028232, 0.4694444444444441089, -0.2206173157302028232 ) ) ;
#14012 = CARTESIAN_POINT ( 'NONE',  ( -1.910449006669871087E-17, 4.925777777777777366, -0.3119999999999999996 ) ) ;
#14013 = VECTOR ( 'NONE', #21123, 39.37007874015748854 ) ;
#14014 = CARTESIAN_POINT ( 'NONE',  ( 0.1993543840281267465, 4.262583333409199149, 0.1993543840281266633 ) ) ;
#14015 = CARTESIAN_POINT ( 'NONE',  ( -0.2819296736111110424, 4.036888888964754507, 0.1167790944451424923 ) ) ;
#14016 = LINE ( 'NONE', #17914, #15135 ) ;
#14017 = CARTESIAN_POINT ( 'NONE',  ( -0.2727340197566736069, 0.3838028176415902437, 0.4171892680188218905 ) ) ;
#14018 = DIRECTION ( 'NONE',  ( 0.2492442549762389770, 0.5597738724868880356, -0.7902724296357380718 ) ) ;
#14019 = ORIENTED_EDGE ( 'NONE', *, *, #20031, .T. ) ;
#14020 = VERTEX_POINT ( 'NONE', #1109 ) ;
#14021 = ORIENTED_EDGE ( 'NONE', *, *, #18698, .F. ) ;
#14022 = CARTESIAN_POINT ( 'NONE',  ( -0.1917385696898717407, 3.994101739603878265, -0.2494960598862051016 ) ) ;
#14023 = CARTESIAN_POINT ( 'NONE',  ( -0.2819296736111110424, 4.460500000075867000, -0.1167790944451423119 ) ) ;
#14024 = CARTESIAN_POINT ( 'NONE',  ( 2.326421213736078119E-17, 0.01160714275960046671, -0.3799334167787516980 ) ) ;
#14025 = CARTESIAN_POINT ( 'NONE',  ( -0.02639353809836864767, 4.515333978748262034, 0.3108816215404409111 ) ) ;
#14026 = CALENDAR_DATE ( 2026, 7, 10 ) ;
#14027 = CARTESIAN_POINT ( 'NONE',  ( -0.4796774085936771903, 0.08639205856936141292, 0.07156340032552072072 ) ) ;
#14028 = CARTESIAN_POINT ( 'NONE',  ( -0.2764156081756484196, 1.692557448933383907E-17, -0.02277777777777679341 ) ) ;
#14029 = AXIS2_PLACEMENT_3D ( 'NONE', #23352, #8487, #13758 ) ;
#14030 = CARTESIAN_POINT ( 'NONE',  ( 5.178964085587577574E-17, 4.158416666742532186, 0.2819296736111110979 ) ) ;
#14031 = DIRECTION ( 'NONE',  ( -0.000000000000000000, -1.000000000000000000, -0.000000000000000000 ) ) ;
#14032 = CC_DESIGN_PERSON_AND_ORGANIZATION_ASSIGNMENT ( #12328, #10606, ( #19646 ) ) ;
#14033 = CARTESIAN_POINT ( 'NONE',  ( 0.1954553509668047195, 0.1954553509668046085, 0.1300000000000021694 ) ) ;
#14034 = CARTESIAN_POINT ( 'NONE',  ( 0.2233192592356399164, 0.1437499999024575703, 0.3073725909049500604 ) ) ;
#14035 = CARTESIAN_POINT ( 'NONE',  ( -0.1167790944451424368, 0.1291666665908000611, 0.2819296736111110424 ) ) ;
#14036 = CARTESIAN_POINT ( 'NONE',  ( 0.4805070082343983473, 0.2560807851245831546, 0.04413116910601659615 ) ) ;
#14037 = CARTESIAN_POINT ( 'NONE',  ( -5.731347020009612645E-17, 0.4486111111111107386, 0.3119999999999999996 ) ) ;
#14038 = CARTESIAN_POINT ( 'NONE',  ( -0.02441201398334213318, 0.9548081934128058723, 3.266702664143262158 ) ) ;
#14039 = LINE ( 'NONE', #19157, #9969 ) ;
#14040 = CARTESIAN_POINT ( 'NONE',  ( -0.1306872919485614903, 0.3155070326520293400, 0.4963194444444493092 ) ) ;
#14041 = CARTESIAN_POINT ( 'NONE',  ( -0.3125000000000000000, 1.913510623667739771E-17, 0.06055555555555702796 ) ) ;
#14042 = CARTESIAN_POINT ( 'NONE',  ( -0.2726133089392542286, 3.775404533184292699, -0.1571433413004071078 ) ) ;
#14043 = CARTESIAN_POINT ( 'NONE',  ( -0.2209708691207961373, -0.2209708691207961095, 0.01194444444444552056 ) ) ;
#14044 = CARTESIAN_POINT ( 'NONE',  ( -0.1993543840281267465, 0.4034722221463555858, 0.1993543840281266633 ) ) ;
#14045 = CARTESIAN_POINT ( 'NONE',  ( 0.1993543840281266633, 4.068138888964754507, -0.1993543840281266910 ) ) ;
#14046 = CARTESIAN_POINT ( 'NONE',  ( 0.2233192592356399997, 0.02232142847388618109, -0.3073725909049500049 ) ) ;
#14047 = CARTESIAN_POINT ( 'NONE',  ( -0.2819296736111110979, 4.755638888964754507, 0.000000000000000000 ) ) ;
#14048 = CARTESIAN_POINT ( 'NONE',  ( 0.3065813772506288948, 5.131179073402218016, -0.008293487530610424083 ) ) ;
#14049 = CARTESIAN_POINT ( 'NONE',  ( 0.2472629257724013041, 5.084277803960305597, -0.1904837651393340436 ) ) ;
#14050 = VECTOR ( 'NONE', #13449, 39.37007874015748143 ) ;
#14051 = ORIENTED_EDGE ( 'NONE', *, *, #14992, .T. ) ;
#14052 = CYLINDRICAL_SURFACE ( 'NONE', #1162, 0.3119999999999999996 ) ;
#14053 = CARTESIAN_POINT ( 'NONE',  ( -0.2206173157302027676, 3.842444444596176290, 0.2206173157302028787 ) ) ;
#14054 = CARTESIAN_POINT ( 'NONE',  ( 5.731347020009612645E-17, 5.064666666666665762, 0.3119999999999999996 ) ) ;
#14055 = ADVANCED_FACE ( 'NONE', ( #8543 ), #18963, .T. ) ;
#14056 = ORIENTED_EDGE ( 'NONE', *, *, #3010, .T. ) ;
#14057 = CARTESIAN_POINT ( 'NONE',  ( -0.1993543840281266910, 4.790361111186976828, -0.1993543840281266910 ) ) ;
#14058 = APPROVAL_STATUS ( 'not_yet_approved' ) ;
#14059 = ADVANCED_FACE ( 'NONE', ( #18533 ), #6636, .F. ) ;
#14060 = DIRECTION ( 'NONE',  ( 0.5643569814744680002, 0.7585083585221992220, 0.3258316551733211330 ) ) ;
#14061 = CARTESIAN_POINT ( 'NONE',  ( 1.910449006669871087E-17, 0.1916666665149337478, -0.3119999999999999996 ) ) ;
#14062 = ORIENTED_EDGE ( 'NONE', *, *, #1736, .F. ) ;
#14063 = CARTESIAN_POINT ( 'NONE',  ( 0.2819296736111110424, 0.1013888888130222432, 0.1167790944451424923 ) ) ;
#14064 = VECTOR ( 'NONE', #18030, 39.37007874015748854 ) ;
#14065 = ORIENTED_EDGE ( 'NONE', *, *, #21743, .T. ) ;
#14066 = DIRECTION ( 'NONE',  ( 0.8651979924482661177, -0.04370253788966846353, 0.4995222938423190540 ) ) ;
#14067 = CARTESIAN_POINT ( 'NONE',  ( -0.6391249999999999432, 3.738758431839877614E-19, 0.000000000000000000 ) ) ;
#14068 = CARTESIAN_POINT ( 'NONE',  ( -0.5116234456863466562, 2.661589509557314326, 2.693707776877850790 ) ) ;
#14069 = CARTESIAN_POINT ( 'NONE',  ( -0.2233192592356399997, 0.1830357141881718830, 0.3073725909049499494 ) ) ;
#14070 = CARTESIAN_POINT ( 'NONE',  ( -0.2904724470272674886, 5.054419505141493296, -0.1139996456453155477 ) ) ;
#14071 = CARTESIAN_POINT ( 'NONE',  ( 0.000000000000000000, 5.384999999999999787, 0.000000000000000000 ) ) ;
#14072 = CARTESIAN_POINT ( 'NONE',  ( 1.964916176665831848, 2.661358883302036293, -1.862525463909579626 ) ) ;
#14073 = CARTESIAN_POINT ( 'NONE',  ( 0.2819296736111110979, 3.877166666742531742, 0.1167790944451422425 ) ) ;
#14074 = DIRECTION ( 'NONE',  ( 0.5773502691896215122, 0.5773502691896279515, 0.5773502691896278405 ) ) ;
#14075 = CARTESIAN_POINT ( 'NONE',  ( 0.2639837978753995507, 0.06059161645832044502, 0.1650549759726013255 ) ) ;
#14076 = CARTESIAN_POINT ( 'NONE',  ( -0.4000000000000000222, 0.2160714283763437438, 0.1299678784931624920 ) ) ;
#14077 = CARTESIAN_POINT ( 'NONE',  ( -0.2206173157302028232, 4.495222222373953969, -0.2206173157302028232 ) ) ;
#14078 = CARTESIAN_POINT ( 'NONE',  ( -0.2819296736111110979, 4.752166666742531298, -0.1167790944451422980 ) ) ;
#14079 = ADVANCED_FACE ( 'NONE', ( #2068 ), #22188, .T. ) ;
#14080 = ORIENTED_EDGE ( 'NONE', *, *, #562, .F. ) ;
#14081 = CARTESIAN_POINT ( 'NONE',  ( 0.1993543840281266633, 4.054250000075865223, -0.1993543840281266910 ) ) ;
#14082 = EDGE_CURVE ( 'NONE', #14348, #11367, #15403, .T. ) ;
#14083 = EDGE_LOOP ( 'NONE', ( #23370, #5627, #14585, #8079 ) ) ;
#14084 = ORIENTED_EDGE ( 'NONE', *, *, #9762, .F. ) ;
#14085 = EDGE_LOOP ( 'NONE', ( #12465, #3952, #12878, #9266 ) ) ;
#14086 = CALENDAR_DATE ( 2026, 7, 10 ) ;
#14087 = EDGE_CURVE ( 'NONE', #9930, #4893, #21446, .T. ) ;
#14088 = CARTESIAN_POINT ( 'NONE',  ( 0.000000000000000000, 0.000000000000000000, 1.326383476483184332 ) ) ;
#14089 = LINE ( 'NONE', #8600, #13966 ) ;
#14090 = CARTESIAN_POINT ( 'NONE',  ( -5.731347020009612645E-17, 0.1083333331816004053, 0.3119999999999999996 ) ) ;
#14091 = DIRECTION ( 'NONE',  ( -0.000000000000000000, -1.000000000000000000, -0.000000000000000000 ) ) ;
#14092 = CARTESIAN_POINT ( 'NONE',  ( -0.4584471372235523479, -0.2219236676878912906, 0.4063138784971527251 ) ) ;
#14093 = PLANE ( 'NONE',  #1897 ) ;
#14094 = VERTEX_POINT ( 'NONE', #1594 ) ;
#14095 = EDGE_LOOP ( 'NONE', ( #3738, #21275, #15996, #13246, #19535 ) ) ;
#14096 = LINE ( 'NONE', #6898, #20854 ) ;
#14097 = FACE_BOUND ( 'NONE', #2497, .T. ) ;
#14098 = CARTESIAN_POINT ( 'NONE',  ( -0.1954553509668046640, 0.1954553509668046918, -0.02972222222222128257 ) ) ;
#14099 = ORIENTED_EDGE ( 'NONE', *, *, #21909, .T. ) ;
#14100 = CARTESIAN_POINT ( 'NONE',  ( 0.1167790944451422702, 4.446611111186975940, -0.2819296736111110424 ) ) ;
#14101 = CARTESIAN_POINT ( 'NONE',  ( 0.1976201361917928889, 0.2172293928240130179, -0.08221809433988200300 ) ) ;
#14102 = CARTESIAN_POINT ( 'NONE',  ( -0.1580085009183549993, 0.7453923191467759501, -1.080137057852694538 ) ) ;
#14103 = DIRECTION ( 'NONE',  ( -0.000000000000000000, -1.000000000000000000, -0.000000000000000000 ) ) ;
#14104 = CARTESIAN_POINT ( 'NONE',  ( -5.731347020009612645E-17, 0.4416666665149336923, 0.3119999999999999996 ) ) ;
#14105 = CARTESIAN_POINT ( 'NONE',  ( 0.2206173157302028787, 3.960499999999999243, 0.2206173157302027954 ) ) ;
#14106 = CARTESIAN_POINT ( 'NONE',  ( 0.2206173157302028787, 5.071611111111109516, 0.2206173157302027954 ) ) ;
#14107 = CARTESIAN_POINT ( 'NONE',  ( 0.3107178308811224254, 4.973614215416888307, 0.02829828600566403063 ) ) ;
#14108 = EDGE_CURVE ( 'NONE', #13469, #5331, #9029, .T. ) ;
#14109 = CARTESIAN_POINT ( 'NONE',  ( 0.000000000000000000, 0.8949999999999999067, 1.015181661097394050 ) ) ;
#14110 = ORIENTED_EDGE ( 'NONE', *, *, #1036, .F. ) ;
#14111 = CARTESIAN_POINT ( 'NONE',  ( -0.1864835714138413370, 4.882863081058048671, -0.2501521505361365971 ) ) ;
#14112 = CARTESIAN_POINT ( 'NONE',  ( -0.4500000000000003997, 0.2598076211353315124, 0.3779506566538943790 ) ) ;
#14113 = CARTESIAN_POINT ( 'NONE',  ( -0.2230971623002954152, -0.2230971623002953874, -0.03840277777777671014 ) ) ;
#14114 = DIRECTION ( 'NONE',  ( 0.000000000000000000, 0.000000000000000000, 1.000000000000000000 ) ) ;
#14115 =( BOUNDED_CURVE ( )  B_SPLINE_CURVE ( 2, ( #21109, #744, #23158, #6350, #13800, #21231, #12106, #983, #10148 ),
 .UNSPECIFIED., .F., .F. ) 
 B_SPLINE_CURVE_WITH_KNOTS ( ( 3, 2, 2, 2, 3 ),
 ( 0.5089285714285716189, 0.5133928571428572063, 0.5178571428571429047, 0.5223214285714284921, 0.5267857142857140795 ),
 .UNSPECIFIED. ) 
 CURVE ( )  GEOMETRIC_REPRESENTATION_ITEM ( )  RATIONAL_B_SPLINE_CURVE ( ( 0.9999999999999962252, 0.9238795325112905132, 1.000000000000000000, 0.9238795325112867385, 1.000000000000000000, 0.9238795325112867385, 1.000000000000000000, 0.9238795325112905132, 0.9999999999999962252 ) ) 
 REPRESENTATION_ITEM ( '' )  );
#14116 = CIRCLE ( 'NONE', #12565, 0.3119999999999999996 ) ;
#14117 = CARTESIAN_POINT ( 'NONE',  ( 0.3038789596872260024, 3.809946929045645359, -0.08166725170457082850 ) ) ;
#14118 = CARTESIAN_POINT ( 'NONE',  ( 0.2233192592356399164, 0.1258928570453146933, 0.3073725909049500604 ) ) ;
#14119 = DIRECTION ( 'NONE',  ( 0.8660254037844384856, 0.000000000000000000, 0.5000000000000003331 ) ) ;
#14120 = CARTESIAN_POINT ( 'NONE',  ( 0.1144950937579609085, -0.2764156081756484751, -0.05402777777777704321 ) ) ;
#14121 = FACE_OUTER_BOUND ( 'NONE', #18554, .T. ) ;
#14122 = CARTESIAN_POINT ( 'NONE',  ( -0.1993543840281266910, 5.082027777853643791, -0.1993543840281266910 ) ) ;
#14123 = CARTESIAN_POINT ( 'NONE',  ( 0.1954553509668047195, 0.1954553509668046085, 0.3522222222222262111 ) ) ;
#14124 = ORIENTED_EDGE ( 'NONE', *, *, #2023, .F. ) ;
#14125 = CARTESIAN_POINT ( 'NONE',  ( -0.001169892149794590427, 4.599422744928899576, -0.3120000010507765764 ) ) ;
#14126 = CARTESIAN_POINT ( 'NONE',  ( 4.113055369932088708E-16, 0.09642857142857140518, 0.4000000000000000222 ) ) ;
#14127 = LINE ( 'NONE', #14248, #16855 ) ;
#14128 = CARTESIAN_POINT ( 'NONE',  ( 0.1292346314604057023, 0.5076388888888885287, 0.3119999999999998885 ) ) ;
#14129 = CARTESIAN_POINT ( 'NONE',  ( -1.910449006669871087E-17, 4.870222222222222008, -0.3119999999999999996 ) ) ;
#14130 = CARTESIAN_POINT ( 'NONE',  ( -0.1993543840281266355, 4.193138888964754507, 0.1993543840281267465 ) ) ;
#14131 = CARTESIAN_POINT ( 'NONE',  ( -0.1167790944451423257, 3.911888888964754507, -0.2819296736111110424 ) ) ;
#14132 = LINE ( 'NONE', #4853, #6130 ) ;
#14133 = CARTESIAN_POINT ( 'NONE',  ( -0.1959149649064394760, 0.4281543196382655569, 0.4181366382341982213 ) ) ;
#14134 = CARTESIAN_POINT ( 'NONE',  ( 1.573500000000000343, 2.683750000000000746, -1.412500000000000089 ) ) ;
#14135 = CARTESIAN_POINT ( 'NONE',  ( 0.000000000000000000, 0.3125000000000000000, 0.1091666666666688823 ) ) ;
#14136 = CARTESIAN_POINT ( 'NONE',  ( 0.2819296736111110979, 4.432722222298088433, 0.1167790944451422425 ) ) ;
#14137 = AXIS2_PLACEMENT_3D ( 'NONE', #8480, #19703, #8357 ) ;
#14138 = CARTESIAN_POINT ( 'NONE',  ( -0.08608376305752644952, 4.490775599581271926, -0.3006775868009963215 ) ) ;
#14139 = EDGE_CURVE ( 'NONE', #2535, #9833, #9146, .T. ) ;
#14140 = APPROVAL_STATUS ( 'not_yet_approved' ) ;
#14141 = CARTESIAN_POINT ( 'NONE',  ( -0.4687500000000003331, -0.04362952321592657862, 0.07944747088523676504 ) ) ;
#14142 = CARTESIAN_POINT ( 'NONE',  ( -0.2764156081756484196, -0.1144950937579609362, -0.07486111111111054539 ) ) ;
#14143 = CARTESIAN_POINT ( 'NONE',  ( -0.2819296736111110979, 4.196611111186976828, -0.1167790944451422980 ) ) ;
#14144 = CONTEXT_DEPENDENT_SHAPE_REPRESENTATION ( #9351, #20448 ) ;
#14145 = CARTESIAN_POINT ( 'NONE',  ( -0.2206173157302027954, 0.3722222222222218990, -0.2206173157302028232 ) ) ;
#14146 = DIRECTION ( 'NONE',  ( 0.000000000000000000, 0.000000000000000000, 1.000000000000000000 ) ) ;
#14147 = CARTESIAN_POINT ( 'NONE',  ( -0.1954553509668046918, -0.1954553509668046640, 0.2688888888888921747 ) ) ;
#14148 = CARTESIAN_POINT ( 'NONE',  ( 0.2233192592356399164, 0.07232142847388617346, 0.3073725909049500604 ) ) ;
#14149 = CARTESIAN_POINT ( 'NONE',  ( -0.1167790944451424368, 0.01805555547968892838, 0.2819296736111110424 ) ) ;
#14150 = CARTESIAN_POINT ( 'NONE',  ( -0.2573004767273367466, 0.1442547113246396839, 0.4064935863995496335 ) ) ;
#14151 = CARTESIAN_POINT ( 'NONE',  ( -0.2206173157302027954, 0.09444444444444409503, -0.2206173157302028232 ) ) ;
#14152 = CARTESIAN_POINT ( 'NONE',  ( -0.1586325827338088967, 0.4496793130216642509, 0.08858683671056809261 ) ) ;
#14153 = CARTESIAN_POINT ( 'NONE',  ( -0.1954553509668046918, -0.1954553509668046640, 0.03972222222222369925 ) ) ;
#14154 = CARTESIAN_POINT ( 'NONE',  ( 0.3155070326520292290, 0.1306872919485615736, 0.4268750000000043898 ) ) ;
#14155 = AXIS2_PLACEMENT_3D ( 'NONE', #23028, #11966, #8154 ) ;
#14156 = ORIENTED_EDGE ( 'NONE', *, *, #21540, .F. ) ;
#14157 = LINE ( 'NONE', #12347, #9098 ) ;
#14158 = CARTESIAN_POINT ( 'NONE',  ( -0.0003064590024795931108, 3.766063790100582231, -0.3119998596873261865 ) ) ;
#14159 = DIRECTION ( 'NONE',  ( 0.5773502691896256200, 0.5773502691896259531, 0.5773502691896256200 ) ) ;
#14160 = CARTESIAN_POINT ( 'NONE',  ( 0.1993543840281266355, 0.3618055554796889006, 0.1993543840281267465 ) ) ;
#14161 = CARTESIAN_POINT ( 'NONE',  ( 0.2819296736111110979, 4.005638888964754507, -3.452642723725051716E-17 ) ) ;
#14162 = CARTESIAN_POINT ( 'NONE',  ( -0.1236067977499790416, 0.4410714283763437216, 0.3804226065180614236 ) ) ;
#14163 = ORIENTED_EDGE ( 'NONE', *, *, #5739, .F. ) ;
#14164 = CARTESIAN_POINT ( 'NONE',  ( -0.1167790944451423257, 4.634111111186976828, -0.2819296736111110424 ) ) ;
#14165 = CARTESIAN_POINT ( 'NONE',  ( 0.2967394294427592727, 5.128870701040007418, 0.08104332260532720600 ) ) ;
#14166 = CARTESIAN_POINT ( 'NONE',  ( 0.05669741369301228850, 5.090589713294394691, -0.3076489064292024511 ) ) ;
#14167 = ORIENTED_EDGE ( 'NONE', *, *, #14489, .F. ) ;
#14168 = CARTESIAN_POINT ( 'NONE',  ( -0.2209708691207961095, 0.2209708691207961373, 0.3938888888888933404 ) ) ;
#14169 = CARTESIAN_POINT ( 'NONE',  ( 0.1993543840281266633, 5.165361111186976828, -0.1993543840281266910 ) ) ;
#14170 = APPROVAL ( #24058, 'UNSPECIFIED' ) ;
#14171 = CARTESIAN_POINT ( 'NONE',  ( 0.3126550460293563427, 4.197112280939127693, -0.01677631843042015625 ) ) ;
#14172 = AXIS2_PLACEMENT_3D ( 'NONE', #3562, #3203, #3092 ) ;
#14173 = CARTESIAN_POINT ( 'NONE',  ( 0.2065212855157302352, 0.03242967361111054325, 0.1924695337126736405 ) ) ;
#14174 = CARTESIAN_POINT ( 'NONE',  ( -1.726321361862525858E-17, 4.783416666742532186, -0.2819296736111110979 ) ) ;
#14175 = COORDINATED_UNIVERSAL_TIME_OFFSET ( 0, 0, .AHEAD. ) ;
#14176 = ORIENTED_EDGE ( 'NONE', *, *, #10045, .T. ) ;
#14177 = CARTESIAN_POINT ( 'NONE',  ( -0.1367999271637809766, 5.104340882757027131, -0.2793827907768540730 ) ) ;
#14178 = ORIENTED_EDGE ( 'NONE', *, *, #22086, .T. ) ;
#14179 = CARTESIAN_POINT ( 'NONE',  ( -0.1167790944451422702, 0.3999999999241333759, -0.2819296736111110424 ) ) ;
#14180 = ORIENTED_EDGE ( 'NONE', *, *, #18271, .T. ) ;
#14181 = CARTESIAN_POINT ( 'NONE',  ( 2.361000000000004206, 0.000000000000000000, -2.201288568297000925 ) ) ;
#14182 = DIRECTION ( 'NONE',  ( -0.9063077870366478273, 0.000000000000000000, -0.4226182617407038267 ) ) ;
#14183 = CARTESIAN_POINT ( 'NONE',  ( 0.2968882310381912304, 4.082774378827750184, 0.09599610789069373817 ) ) ;
#14184 = CARTESIAN_POINT ( 'NONE',  ( 0.2233192592356399997, 0.2187499999024575814, -0.3073725909049500049 ) ) ;
#14185 = CARTESIAN_POINT ( 'NONE',  ( -0.1644747555172010878, 5.066690419149153080, 0.2661110666209607345 ) ) ;
#14186 = EDGE_CURVE ( 'NONE', #17972, #5886, #9789, .T. ) ;
#14187 = FACE_OUTER_BOUND ( 'NONE', #1152, .T. ) ;
#14188 = CARTESIAN_POINT ( 'NONE',  ( -0.2819296736111110424, 4.703555555631421470, 0.1167790944451424923 ) ) ;
#14189 = CARTESIAN_POINT ( 'NONE',  ( -0.05482473137696326770, -0.5228958406531273306, 0.05347130368200832956 ) ) ;
#14190 = EDGE_CURVE ( 'NONE', #1934, #10834, #17425, .T. ) ;
#14191 = AXIS2_PLACEMENT_3D ( 'NONE', #16869, #278, #157 ) ;
#14192 = CARTESIAN_POINT ( 'NONE',  ( -0.1993543840281266910, 3.734805555631421026, -0.1993543840281266910 ) ) ;
#14193 = DIRECTION ( 'NONE',  ( 0.000000000000000000, 0.000000000000000000, 1.000000000000000000 ) ) ;
#14194 = CARTESIAN_POINT ( 'NONE',  ( 0.07868793315885187767, 5.018292790751019972, 0.3026089890143150440 ) ) ;
#14195 = CARTESIAN_POINT ( 'NONE',  ( 0.1989077834500278252, 5.073000000000000398, 0.2437966507032887920 ) ) ;
#14196 = CARTESIAN_POINT ( 'NONE',  ( -0.06335377612981457629, 0.2285266326068134957, 0.3999999999999999667 ) ) ;
#14197 = CARTESIAN_POINT ( 'NONE',  ( -0.2206173157302027676, 4.398000000151732536, 0.2206173157302028787 ) ) ;
#14198 = EDGE_CURVE ( 'NONE', #5827, #16588, #4492, .T. ) ;
#14199 = CARTESIAN_POINT ( 'NONE',  ( 5.178964085587577574E-17, 4.825083333409199149, 0.2819296736111110979 ) ) ;
#14200 = VERTEX_POINT ( 'NONE', #4371 ) ;
#14201 = CIRCLE ( 'NONE', #6408, 0.001000000000000003057 ) ;
#14202 = CARTESIAN_POINT ( 'NONE',  ( -0.1167790944451423257, 4.009111111186976828, -0.2819296736111110424 ) ) ;
#14203 = PRODUCT_DEFINITION_SHAPE ( 'NONE', 'NONE',  #2989 ) ;
#14204 = EDGE_LOOP ( 'NONE', ( #15290, #96 ) ) ;
#14205 = COORDINATED_UNIVERSAL_TIME_OFFSET ( 0, 0, .AHEAD. ) ;
#14206 = AXIS2_PLACEMENT_3D ( 'NONE', #5559, #3737, #16545 ) ;
#14207 = CARTESIAN_POINT ( 'NONE',  ( 0.4678785457174672868, 0.2663437566607212981, 0.05892894635879551701 ) ) ;
#14208 = CARTESIAN_POINT ( 'NONE',  ( 1.145733547534701715E-12, 5.130222168000691418, 0.3067077167097377322 ) ) ;
#14209 = ORIENTED_EDGE ( 'NONE', *, *, #12758, .F. ) ;
#14210 = CARTESIAN_POINT ( 'NONE',  ( 0.1292346314604056745, 0.1881944442927115102, -0.3119999999999999996 ) ) ;
#14211 = CARTESIAN_POINT ( 'NONE',  ( -0.2707896025394566086, 4.386469429090337435, -0.1563191200470392395 ) ) ;
#14212 = CARTESIAN_POINT ( 'NONE',  ( -0.4687500000000003886, -0.08852780644244462316, 0.4134630671871108443 ) ) ;
#14213 = VERTEX_POINT ( 'NONE', #11467 ) ;
#14214 = APPROVAL_PERSON_ORGANIZATION ( #10252, #3590, #22922 ) ;
#14215 = CARTESIAN_POINT ( 'NONE',  ( 0.3119999999999999996, 0.2368055554038226151, -0.1292346314604056468 ) ) ;
#14216 = CARTESIAN_POINT ( 'NONE',  ( 1.726321361862525858E-17, 0.04930555547968892144, -0.2819296736111110979 ) ) ;
#14217 = CARTESIAN_POINT ( 'NONE',  ( -0.1954553509668046918, -0.1954553509668046640, -0.01583333333333228690 ) ) ;
#14218 = CARTESIAN_POINT ( 'NONE',  ( 0.1167790944451424368, 4.481333333409199149, 0.2819296736111110424 ) ) ;
#14219 = CARTESIAN_POINT ( 'NONE',  ( 0.09987075367823565475, 0.2738295200956132880, -0.08002286816158230009 ) ) ;
#14220 = CARTESIAN_POINT ( 'NONE',  ( -0.04142811702957077680, 0.7863941770016692479, -1.079911001309288299 ) ) ;
#14221 = CARTESIAN_POINT ( 'NONE',  ( 0.3125000000000000000, -5.740531871003217465E-17, -0.02277777777777697382 ) ) ;
#14222 = LINE ( 'NONE', #2874, #15115 ) ;
#14223 = CARTESIAN_POINT ( 'NONE',  ( 0.3119999999999999996, 3.967444444444443441, -3.820898013339742174E-17 ) ) ;
#14224 = CARTESIAN_POINT ( 'NONE',  ( 0.3124999999999989453, 0.1294417382415933571, 0.1473611111111133576 ) ) ;
#14225 = AXIS2_PLACEMENT_3D ( 'NONE', #9132, #20474, #3770 ) ;
#14226 = ADVANCED_FACE ( 'NONE', ( #8146 ), #8182, .F. ) ;
#14227 = CARTESIAN_POINT ( 'NONE',  ( 0.3042924909783515930, 4.972423745096966385, 0.06982855329471476802 ) ) ;
#14228 = CARTESIAN_POINT ( 'NONE',  ( -0.3125000000000010547, 0.1294417382415911921, 0.2237500000000028078 ) ) ;
#14229 = APPROVAL_PERSON_ORGANIZATION ( #7132, #16403, #9071 ) ;
#14230 = CARTESIAN_POINT ( 'NONE',  ( 0.3125000000000004996, 0.1294417382415917750, 0.2098611111111141347 ) ) ;
#14231 = CARTESIAN_POINT ( 'NONE',  ( 0.3155070326520292290, -0.1306872919485616569, -0.02104166666666545948 ) ) ;
#14232 = CARTESIAN_POINT ( 'NONE',  ( -0.3613381517857143232, 0.3294642856167431799, -0.1174058825155741004 ) ) ;
#14233 = AXIS2_PLACEMENT_3D ( 'NONE', #17875, #13861, #23336 ) ;
#14234 = CARTESIAN_POINT ( 'NONE',  ( 0.3120000192078950518, 3.808819556236046733, -0.04084196867937928827 ) ) ;
#14235 = ADVANCED_FACE ( 'NONE', ( #15598 ), #22906, .F. ) ;
#14236 = CARTESIAN_POINT ( 'NONE',  ( 0.2923287055106771337, 0.2723214284738861291, 0.2123892367102621359 ) ) ;
#14237 = EDGE_CURVE ( 'NONE', #23116, #13196, #15541, .T. ) ;
#14238 = EDGE_CURVE ( 'NONE', #363, #6320, #6201, .T. ) ;
#14239 = CARTESIAN_POINT ( 'NONE',  ( -5.178964085587577574E-17, 0.03541666659080003332, 0.2819296736111110979 ) ) ;
#14240 = CARTESIAN_POINT ( 'NONE',  ( 0.1144950937579609085, -0.2764156081756484751, 0.001527777777778949230 ) ) ;
#14241 = CARTESIAN_POINT ( 'NONE',  ( 0.4801334617939588822, -0.2624565244266456876, 0.04287645741408795813 ) ) ;
#14242 = FACE_OUTER_BOUND ( 'NONE', #6897, .T. ) ;
#14243 = CARTESIAN_POINT ( 'NONE',  ( 0.2764156081756483641, -0.1144950937579611167, 0.3973611111111153837 ) ) ;
#14244 = ORIENTED_EDGE ( 'NONE', *, *, #19446, .F. ) ;
#14245 = CARTESIAN_POINT ( 'NONE',  ( -0.1749087105507561857, 4.604688012726042778, -0.2584107560775423806 ) ) ;
#14246 = CARTESIAN_POINT ( 'NONE',  ( -0.3055012760687011442, 4.277984914513297099, -0.06818561754197617619 ) ) ;
#14247 = DIRECTION ( 'NONE',  ( 0.000000000000000000, 1.000000000000000000, 0.000000000000000000 ) ) ;
#14248 = CARTESIAN_POINT ( 'NONE',  ( 2.556721741255282954, 0.000000000000000000, -2.088288568297006265 ) ) ;
#14249 = CARTESIAN_POINT ( 'NONE',  ( -0.2206173157302028787, 0.4416666666666662633, 0.2206173157302027954 ) ) ;
#14250 = CARTESIAN_POINT ( 'NONE',  ( 0.2206173157302027954, 4.752166666666665762, -0.2206173157302028232 ) ) ;
#14251 = CARTESIAN_POINT ( 'NONE',  ( -0.2819296736111110424, 4.300777777853643791, 0.1167790944451424923 ) ) ;
#14252 = PLANE ( 'NONE',  #9714 ) ;
#14253 = EDGE_CURVE ( 'NONE', #7960, #1032, #1960, .T. ) ;
#14254 = DIRECTION ( 'NONE',  ( -0.8660254037844434816, 0.000000000000000000, -0.4999999999999913403 ) ) ;
#14255 = ORIENTED_EDGE ( 'NONE', *, *, #7472, .F. ) ;
#14256 = CIRCLE ( 'NONE', #3354, 0.01874999999999999237 ) ;
#14257 = DIRECTION ( 'NONE',  ( 1.224646799147352221E-16, 0.000000000000000000, -1.000000000000000000 ) ) ;
#14258 = CARTESIAN_POINT ( 'NONE',  ( 0.2819296736111110424, 4.606333333409200037, -0.1167790944451423396 ) ) ;
#14259 = CARTESIAN_POINT ( 'NONE',  ( 0.2658399375774659346, -0.1645562284175245416, 0.4238565772525364483 ) ) ;
#14260 = CARTESIAN_POINT ( 'NONE',  ( 0.4620775622572421693, -0.2744852724095710461, 0.05975564523638850906 ) ) ;
#14261 = PERSON_AND_ORGANIZATION ( #15518, #2538 ) ;
#14262 = CYLINDRICAL_SURFACE ( 'NONE', #8794, 0.3119999999999999996 ) ;
#14263 = CARTESIAN_POINT ( 'NONE',  ( 0.2764156081756483641, 0.1144950937579610056, 0.008472222222223456389 ) ) ;
#14264 = CARTESIAN_POINT ( 'NONE',  ( 0.1167790944451422702, 4.182722222298088433, -0.2819296736111110979 ) ) ;
#14265 = CARTESIAN_POINT ( 'NONE',  ( -0.0002601744550385995803, 4.821618687316853169, -0.3120000001095587505 ) ) ;
#14266 = CARTESIAN_POINT ( 'NONE',  ( 5.731347020009612645E-17, 4.897999999999998799, 0.3119999999999999996 ) ) ;
#14267 = CARTESIAN_POINT ( 'NONE',  ( 0.2764156081756483641, -0.1144950937579611028, 0.2862500000000034461 ) ) ;
#14268 = CARTESIAN_POINT ( 'NONE',  ( -0.2233192592356399442, 0.1080357141881718719, -0.3073725909049500049 ) ) ;
#14269 = VECTOR ( 'NONE', #19235, 39.37007874015748143 ) ;
#14270 = CARTESIAN_POINT ( 'NONE',  ( 0.2819296736111110424, 0.03194444436857781650, 0.1167790944451424923 ) ) ;
#14271 = FACE_OUTER_BOUND ( 'NONE', #17955, .T. ) ;
#14272 = DIRECTION ( 'NONE',  ( 0.000000000000000000, 0.000000000000000000, -1.000000000000000000 ) ) ;
#14273 = CARTESIAN_POINT ( 'NONE',  ( -0.1820207676368335581, 0.4792642385880945821, -0.7276181116126451132 ) ) ;
#14274 = CARTESIAN_POINT ( 'NONE',  ( -0.1954553509668046640, 0.1954553509668046918, -0.02972222222222128257 ) ) ;
#14275 = CARTESIAN_POINT ( 'NONE',  ( 0.2230971623002954429, 0.2230971623002953319, 0.4303472222222265997 ) ) ;
#14276 = ORIENTED_EDGE ( 'NONE', *, *, #16478, .F. ) ;
#14277 = CARTESIAN_POINT ( 'NONE',  ( -0.2472135954999579444, 0.06785714285714283811, -0.3402603233408160732 ) ) ;
#14278 = CARTESIAN_POINT ( 'NONE',  ( 0.3125000000000007772, -0.1294417382415915807, 0.02930555555555680591 ) ) ;
#14279 = CARTESIAN_POINT ( 'NONE',  ( -0.1167790944451422702, 0.3861111110352444808, -0.2819296736111110424 ) ) ;
#14280 = CARTESIAN_POINT ( 'NONE',  ( 0.2819296736111110979, 3.950083333409199149, -3.452642723725051716E-17 ) ) ;
#14281 = CARTESIAN_POINT ( 'NONE',  ( 0.1116596296178199860, -0.04553571438325666743, -0.3436530038418508792 ) ) ;
#14282 = ADVANCED_FACE ( 'NONE', ( #19248 ), #791, .F. ) ;
#14283 = VERTEX_POINT ( 'NONE', #2553 ) ;
#14284 = CARTESIAN_POINT ( 'NONE',  ( 0.1167790944451422702, 4.738277777853642903, -0.2819296736111110424 ) ) ;
#14285 = DIRECTION ( 'NONE',  ( 0.000000000000000000, 0.000000000000000000, -1.000000000000000000 ) ) ;
#14286 =( BOUNDED_CURVE ( )  B_SPLINE_CURVE ( 2, ( #5230, #21820, #3285, #18169, #10860, #18289, #1465, #9022, #8024, #13661, #17059, #22424, #16827 ),
 .UNSPECIFIED., .F., .F. ) 
 B_SPLINE_CURVE_WITH_KNOTS ( ( 3, 2, 2, 2, 2, 2, 3 ),
 ( 0.1071428571428571508, 0.1142857142857142821, 0.1285714285714285587, 0.1428571428571428492, 0.1571428571428571397, 0.1714285714285714302, 0.1785714285714285754 ),
 .UNSPECIFIED. ) 
 CURVE ( )  GEOMETRIC_REPRESENTATION_ITEM ( )  RATIONAL_B_SPLINE_CURVE ( ( 0.9755282581475768211, 0.9755282581475768211, 1.000000000000000000, 0.9510565162951535312, 1.000000000000000000, 0.9510565162951535312, 1.000000000000000000, 0.9510565162951535312, 1.000000000000000000, 0.9510565162951535312, 1.000000000000000000, 0.9755282581475768211, 0.9755282581475768211 ) ) 
 REPRESENTATION_ITEM ( '' )  );
#14287 = DIRECTION ( 'NONE',  ( -0.000000000000000000, -1.000000000000000000, -0.000000000000000000 ) ) ;
#14288 = ORIENTED_EDGE ( 'NONE', *, *, #18638, .F. ) ;
#14289 = FACE_OUTER_BOUND ( 'NONE', #17475, .T. ) ;
#14290 = CARTESIAN_POINT ( 'NONE',  ( -0.1167790944451423257, 5.064666666742533074, -0.2819296736111110424 ) ) ;
#14291 = CARTESIAN_POINT ( 'NONE',  ( 0.04350585610265966102, 4.209263110863878055, -0.3090598294826615300 ) ) ;
#14292 = VECTOR ( 'NONE', #1817, 39.37007874015748143 ) ;
#14293 =( LENGTH_UNIT ( ) NAMED_UNIT ( * ) SI_UNIT ( $, .METRE. ) );
#14294 = ORIENTED_EDGE ( 'NONE', *, *, #20324, .T. ) ;
#14295 = CARTESIAN_POINT ( 'NONE',  ( 0.1334304699324121435, 5.206640035683670398, 0.2489627644214695845 ) ) ;
#14296 = CARTESIAN_POINT ( 'NONE',  ( 0.2819296736111110979, 4.828555555631420582, -0.1167790944451423396 ) ) ;
#14297 = DATE_AND_TIME ( #18068, #6460 ) ;
#14298 = ORIENTED_EDGE ( 'NONE', *, *, #17942, .T. ) ;
#14299 = DIRECTION ( 'NONE',  ( -0.000000000000000000, -1.000000000000000000, -0.000000000000000000 ) ) ;
#14300 = CARTESIAN_POINT ( 'NONE',  ( -0.1206839867636108760, 4.568140654558272118, 0.2884027983365602954 ) ) ;
#14301 = ORIENTED_EDGE ( 'NONE', *, *, #22714, .F. ) ;
#14302 = CARTESIAN_POINT ( 'NONE',  ( 0.2819296736111110424, 0.2680555554796889561, 0.1167790944451424923 ) ) ;
#14303 = VERTEX_POINT ( 'NONE', #18899 ) ;
#14304 = CARTESIAN_POINT ( 'NONE',  ( -0.2819296736111110979, 0.02152777770191114520, -3.452642723725051716E-17 ) ) ;
#14305 = CARTESIAN_POINT ( 'NONE',  ( -0.03900460988328559309, 4.737132092303641073, 0.3120000036723390435 ) ) ;
#14306 = DIRECTION ( 'NONE',  ( 0.000000000000000000, 0.000000000000000000, 1.000000000000000000 ) ) ;
#14307 = CARTESIAN_POINT ( 'NONE',  ( 0.3999999999999999667, -0.03214285714285715356, 0.1299678784931626307 ) ) ;
#14308 = CARTESIAN_POINT ( 'NONE',  ( -0.2296592410380279836, 5.064312714222578116, 0.2111886365721926673 ) ) ;
#14309 = CARTESIAN_POINT ( 'NONE',  ( 0.2206173157302028787, 4.182722222222221120, 0.2206173157302027954 ) ) ;
#14310 = DIRECTION ( 'NONE',  ( -0.8660254037844437036, 0.000000000000000000, 0.4999999999999913403 ) ) ;
#14311 = CARTESIAN_POINT ( 'NONE',  ( 0.2819296736111110424, 4.842444444520309865, -0.1167790944451423396 ) ) ;
#14312 = VECTOR ( 'NONE', #20034, 39.37007874015748143 ) ;
#14313 = CARTESIAN_POINT ( 'NONE',  ( 0.2811290616301844736, 4.525923312079648042, 0.1368482528082854699 ) ) ;
#14314 = CARTESIAN_POINT ( 'NONE',  ( -0.2819296736111110424, 5.252166666742532186, -0.1167790944451423119 ) ) ;
#14315 = EDGE_CURVE ( 'NONE', #20728, #8276, #16322, .T. ) ;
#14316 = CARTESIAN_POINT ( 'NONE',  ( -0.2922127367187743463, 0.05061570093428138795, -0.07118518849912422453 ) ) ;
#14317 = CARTESIAN_POINT ( 'NONE',  ( 0.3860879860166508970, 0.9548081934128058723, 2.555695807636233496 ) ) ;
#14318 = CARTESIAN_POINT ( 'NONE',  ( -0.4675613926561249523, -0.2849392891917814086, 0.04271845132551763818 ) ) ;
#14319 = CARTESIAN_POINT ( 'NONE',  ( -0.1166234456863465135, 3.066692553488282957, 2.777423565910347225 ) ) ;
#14320 = CARTESIAN_POINT ( 'NONE',  ( -0.3119999999999998885, 4.283416666818398610, 0.1292346314604058410 ) ) ;
#14321 = CARTESIAN_POINT ( 'NONE',  ( 0.2819296736111111534, 4.724388888964754507, 0.1167790944451422563 ) ) ;
#14322 = CARTESIAN_POINT ( 'NONE',  ( 0.1167790944451422702, 3.891055555631421914, -0.2819296736111110424 ) ) ;
#14323 = ORIENTED_EDGE ( 'NONE', *, *, #4532, .F. ) ;
#14324 = EDGE_CURVE ( 'NONE', #16427, #363, #13420, .T. ) ;
#14325 = AXIS2_PLACEMENT_3D ( 'NONE', #21722, #13933, #10279 ) ;
#14326 = COORDINATED_UNIVERSAL_TIME_OFFSET ( 0, 0, .AHEAD. ) ;
#14327 =( BOUNDED_CURVE ( )  B_SPLINE_CURVE ( 2, ( #3, #16843, #20500, #7100, #7451, #11360, #20264, #22444, #14538 ),
 .UNSPECIFIED., .F., .F. ) 
 B_SPLINE_CURVE_WITH_KNOTS ( ( 3, 2, 2, 2, 3 ),
 ( 0.3541666666666666852, 0.3645833333333333148, 0.3750000000000000000, 0.3854166666666666852, 0.3958333333333333148 ),
 .UNSPECIFIED. ) 
 CURVE ( )  GEOMETRIC_REPRESENTATION_ITEM ( )  RATIONAL_B_SPLINE_CURVE ( ( 1.000000000000000000, 0.9238795325112867385, 1.000000000000000000, 0.9238795325112867385, 1.000000000000000000, 0.9238795325112867385, 1.000000000000000000, 0.9238795325112867385, 1.000000000000000000 ) ) 
 REPRESENTATION_ITEM ( '' )  );
#14328 = DIRECTION ( 'NONE',  ( 0.000000000000000000, 0.000000000000000000, -1.000000000000000000 ) ) ;
#14329 = CARTESIAN_POINT ( 'NONE',  ( -0.3124999999999993894, -0.1294417382415926909, 0.2376388888888920914 ) ) ;
#14330 = VERTEX_POINT ( 'NONE', #19020 ) ;
#14331 = CARTESIAN_POINT ( 'NONE',  ( -0.3119999999999999996, 0.2055555554038226151, -3.820898013339742174E-17 ) ) ;
#14332 = CARTESIAN_POINT ( 'NONE',  ( -0.1913778543947200761, 4.399133461649255672, 0.2497584621283620854 ) ) ;
#14333 = CC_DESIGN_DATE_AND_TIME_ASSIGNMENT ( #8314, #15766, ( #16981 ) ) ;
#14334 = CARTESIAN_POINT ( 'NONE',  ( 0.2209708691207961095, -0.2209708691207961651, -0.08527777777777745261 ) ) ;
#14335 = CARTESIAN_POINT ( 'NONE',  ( -0.2472135954999579444, 0.3535714285714284810, -0.3402603233408160732 ) ) ;
#14336 = ORIENTED_EDGE ( 'NONE', *, *, #13407, .T. ) ;
#14337 = FACE_OUTER_BOUND ( 'NONE', #7378, .T. ) ;
#14338 = CARTESIAN_POINT ( 'NONE',  ( 0.1993543840281266355, 0.3618055554796889006, 0.1993543840281267465 ) ) ;
#14339 = CARTESIAN_POINT ( 'NONE',  ( 0.2764156081756483641, 0.1144950937579610056, 0.008472222222223456389 ) ) ;
#14340 = CARTESIAN_POINT ( 'NONE',  ( 5.178964085587577574E-17, 4.422305555631421470, 0.2819296736111110979 ) ) ;
#14341 = CARTESIAN_POINT ( 'NONE',  ( 0.2973707438694047078, 0.01885122216165743478, -0.08653741053607123812 ) ) ;
#14342 = DIRECTION ( 'NONE',  ( 0.000000000000000000, -0.7071067811865489050, -0.7071067811865461294 ) ) ;
#14343 = DIRECTION ( 'NONE',  ( -0.000000000000000000, -1.000000000000000000, -0.000000000000000000 ) ) ;
#14344 = CARTESIAN_POINT ( 'NONE',  ( 0.3119999999999999996, 4.075083333333332725, 0.1292346314604056190 ) ) ;
#14345 = AXIS2_PLACEMENT_3D ( 'NONE', #4426, #17245, #13828 ) ;
#14346 = CARTESIAN_POINT ( 'NONE',  ( 0.3119999999999999996, 4.863277777929510215, -3.820898013339742174E-17 ) ) ;
#14347 = ADVANCED_BREP_SHAPE_REPRESENTATION ( '', ( #17608, #9127 ), #20827 ) ;
#14348 = VERTEX_POINT ( 'NONE', #17189 ) ;
#14349 = CARTESIAN_POINT ( 'NONE',  ( 5.731347020009612645E-17, 4.842444444444443441, 0.3119999999999999996 ) ) ;
#14350 = VERTEX_POINT ( 'NONE', #475 ) ;
#14351 = CARTESIAN_POINT ( 'NONE',  ( -0.04081130781707435068, 4.903883588982272279, 0.3119999910883811123 ) ) ;
#14352 = EDGE_CURVE ( 'NONE', #2478, #5171, #2356, .T. ) ;
#14353 = CARTESIAN_POINT ( 'NONE',  ( 0.2230971623002954429, 0.2230971623002953319, 0.1560416666666692986 ) ) ;
#14354 = CARTESIAN_POINT ( 'NONE',  ( -0.2233192592356399997, 0.4151785713310289783, 0.3073725909049499494 ) ) ;
#14355 = AXIS2_PLACEMENT_3D ( 'NONE', #19038, #16962, #20620 ) ;
#14356 = DIRECTION ( 'NONE',  ( -0.000000000000000000, -0.000000000000000000, 1.000000000000000000 ) ) ;
#14357 = ADVANCED_FACE ( 'NONE', ( #19846, #10235 ), #10476, .T. ) ;
#14358 = CARTESIAN_POINT ( 'NONE',  ( -0.3613381517857143232, 0.2437499999024575481, -4.425116109941954795E-17 ) ) ;
#14359 = CARTESIAN_POINT ( 'NONE',  ( -0.001863919267180048824, -0.003009961218012348859, 2.816660016782450704 ) ) ;
#14360 = CARTESIAN_POINT ( 'NONE',  ( 0.1954553509668047195, 0.1954553509668046085, 0.01888888888889020401 ) ) ;
#14361 = CARTESIAN_POINT ( 'NONE',  ( -0.2819296736111110979, 5.200083333409199149, 0.000000000000000000 ) ) ;
#14362 = CARTESIAN_POINT ( 'NONE',  ( 0.2734354562523998444, 4.478980055100710622, -0.1527955304013648985 ) ) ;
#14363 = ORIENTED_EDGE ( 'NONE', *, *, #9382, .F. ) ;
#14364 = CARTESIAN_POINT ( 'NONE',  ( -0.09885966046364118298, 4.602272359509021804, -0.2966034080420659746 ) ) ;
#14365 = CARTESIAN_POINT ( 'NONE',  ( 0.000000000000000000, 3.659999999999999698, 0.000000000000000000 ) ) ;
#14366 = DIRECTION ( 'NONE',  ( 0.000000000000000000, 0.000000000000000000, 1.000000000000000000 ) ) ;
#14367 = DIRECTION ( 'NONE',  ( -1.707404996040164512E-16, 0.000000000000000000, 1.000000000000000000 ) ) ;
#14368 = CARTESIAN_POINT ( 'NONE',  ( 0.3119999999999999996, 4.804249999999998799, -0.1292346314604056745 ) ) ;
#14369 = B_SPLINE_CURVE_WITH_KNOTS ( 'NONE', 3,
 ( #12710, #18176, #10745, #20005, #3416, #23642, #18295, #8779, #21715, #23520 ),
 .UNSPECIFIED., .F., .F.,
 ( 4, 2, 2, 2, 4 ),
 ( 0.000000000000000000, 0.003270554913819859796, 0.006541109827639719591, 0.009811664741459578953, 0.01308221965527943918 ),
 .UNSPECIFIED. ) ;
#14370 = CARTESIAN_POINT ( 'NONE',  ( 5.178964085587577574E-17, 3.922305555631421026, 0.2819296736111110979 ) ) ;
#14371 = DIRECTION ( 'NONE',  ( 0.000000000000000000, -0.9961946980917454342, -0.08715574274765833240 ) ) ;
#14372 = DIRECTION ( 'NONE',  ( -0.6568875074630621258, 0.6516633103466551447, -0.3792541792610923390 ) ) ;
#14373 = CARTESIAN_POINT ( 'NONE',  ( 0.004187250022457379706, 0.5383673285787200502, 0.04698409998689229844 ) ) ;
#14374 = ORIENTED_EDGE ( 'NONE', *, *, #16191, .F. ) ;
#14375 = AXIS2_PLACEMENT_3D ( 'NONE', #21320, #3380, #16312 ) ;
#14376 = CARTESIAN_POINT ( 'NONE',  ( 0.1292346314604058410, 3.901472222222222008, 0.3119999999999998885 ) ) ;
#14377 = CARTESIAN_POINT ( 'NONE',  ( 0.2819296736111110424, 4.495222222298087544, -0.1167790944451423396 ) ) ;
#14378 = ADVANCED_FACE ( 'NONE', ( #21797 ), #2742, .F. ) ;
#14379 = EDGE_CURVE ( 'NONE', #15066, #6859, #20527, .T. ) ;
#14380 = CARTESIAN_POINT ( 'NONE',  ( -0.2581348291378180448, 4.507463561769111671, 0.1754396708902748736 ) ) ;
#14381 = EDGE_CURVE ( 'NONE', #12247, #18827, #15830, .T. ) ;
#14382 = EDGE_CURVE ( 'NONE', #16112, #6049, #19930, .T. ) ;
#14383 = DATE_AND_TIME ( #12566, #6024 ) ;
#14384 = CARTESIAN_POINT ( 'NONE',  ( 0.000000000000000000, 0.4197679491924312112, 0.000000000000000000 ) ) ;
#14385 = CARTESIAN_POINT ( 'NONE',  ( -0.1954553509668046918, -0.1954553509668046640, -0.07138888888888827999 ) ) ;
#14386 = CARTESIAN_POINT ( 'NONE',  ( 0.1993543840281266633, 4.123694444520309865, -0.1993543840281266910 ) ) ;
#14387 = CARTESIAN_POINT ( 'NONE',  ( 1.910449006669871087E-17, 0.3652777777777774237, -0.3119999999999999996 ) ) ;
#14388 = EDGE_CURVE ( 'NONE', #20417, #8097, #11342, .T. ) ;
#14389 = FACE_OUTER_BOUND ( 'NONE', #10800, .T. ) ;
#14390 = LINE ( 'NONE', #8896, #1126 ) ;
#14391 = CARTESIAN_POINT ( 'NONE',  ( 0.3613381517857143232, 0.01517857133102902024, -0.1174058825155740587 ) ) ;
#14392 = AXIS2_PLACEMENT_3D ( 'NONE', #2446, #3909, #15370 ) ;
#14393 = B_SPLINE_CURVE_WITH_KNOTS ( 'NONE', 3,
 ( #882, #12361, #8672, #13941, #19536, #23537, #14295, #10286, #17709, #13284 ),
 .UNSPECIFIED., .F., .F.,
 ( 4, 2, 2, 2, 4 ),
 ( 0.005993913058028690378, 0.007327704144062629002, 0.008661495230096568493, 0.009995286316130507984, 0.01132907740216444574 ),
 .UNSPECIFIED. ) ;
#14394 = CARTESIAN_POINT ( 'NONE',  ( 0.1993543840281266355, 0.02847222214635558926, 0.1993543840281267465 ) ) ;
#14395 = CARTESIAN_POINT ( 'NONE',  ( 0.4802534502443344122, 0.2139688138246751414, 0.05347119198895301101 ) ) ;
#14396 = CYLINDRICAL_SURFACE ( 'NONE', #275, 0.3119999999999999996 ) ;
#14397 = CARTESIAN_POINT ( 'NONE',  ( -0.1066700245536902208, 0.5609335224602052250, -0.7424636365021335394 ) ) ;
#14398 = CARTESIAN_POINT ( 'NONE',  ( 0.2764156081756483641, 0.1144950937579610195, -0.04708333333333253323 ) ) ;
#14399 = CARTESIAN_POINT ( 'NONE',  ( -0.1306872919485615459, -0.3155070326520293400, 0.4615972222222268218 ) ) ;
#14400 = ORIENTED_EDGE ( 'NONE', *, *, #10374, .T. ) ;
#14401 = EDGE_LOOP ( 'NONE', ( #12875, #19066, #16349, #1028 ) ) ;
#14402 = DIRECTION ( 'NONE',  ( 0.000000000000000000, 0.000000000000000000, -1.000000000000000000 ) ) ;
#14403 = CARTESIAN_POINT ( 'NONE',  ( -0.3120000192244279935, 3.836597312062911325, 0.04084114088547415033 ) ) ;
#14404 = CARTESIAN_POINT ( 'NONE',  ( -0.1167790944451424368, 0.5180555554796888451, 0.2819296736111110424 ) ) ;
#14405 = CARTESIAN_POINT ( 'NONE',  ( -1.726321361862525858E-17, 3.797305555631421470, -0.2819296736111110979 ) ) ;
#14406 = CARTESIAN_POINT ( 'NONE',  ( 0.3613381517857143232, 0.07946428561674330482, 0.1174058825155742114 ) ) ;
#14407 = ORIENTED_EDGE ( 'NONE', *, *, #16857, .F. ) ;
#14408 = CARTESIAN_POINT ( 'NONE',  ( -0.1993543840281266910, 4.470916666742532186, -0.1993543840281266910 ) ) ;
#14409 = PRODUCT ( 'Aloris-BXA-Ball', 'Aloris-BXA-Ball', '', ( #12515 ) ) ;
#14410 = FACE_OUTER_BOUND ( 'NONE', #3313, .T. ) ;
#14411 = LINE ( 'NONE', #10873, #21526 ) ;
#14412 = ORIENTED_EDGE ( 'NONE', *, *, #18402, .F. ) ;
#14413 = CARTESIAN_POINT ( 'NONE',  ( 3.820898013339742174E-17, 5.384999999999999787, 0.3119999999999999996 ) ) ;
#14414 = CARTESIAN_POINT ( 'NONE',  ( -0.1167790944451423257, 5.120222222298088433, -0.2819296736111110424 ) ) ;
#14415 = AXIS2_PLACEMENT_3D ( 'NONE', #20027, #14066, #1495 ) ;
#14416 = CARTESIAN_POINT ( 'NONE',  ( -0.4687500000000003886, 0.2598076211353315124, 0.4425000000000000044 ) ) ;
#14417 = CIRCLE ( 'NONE', #3510, 0.03500000000000003803 ) ;
#14418 = LINE ( 'NONE', #5377, #4517 ) ;
#14419 = CARTESIAN_POINT ( 'NONE',  ( 0.1993543840281267465, 4.818138888964754507, 0.1993543840281266633 ) ) ;
#14420 = CALENDAR_DATE ( 2026, 7, 10 ) ;
#14421 = ORIENTED_EDGE ( 'NONE', *, *, #16816, .T. ) ;
#14422 = ADVANCED_FACE ( 'NONE', ( #20095 ), #18383, .T. ) ;
#14423 = PLANE ( 'NONE',  #1985 ) ;
#14424 = CARTESIAN_POINT ( 'NONE',  ( -0.01848103877824625041, 0.5441716683897389606, 0.04413116910601661003 ) ) ;
#14425 = ORIENTED_EDGE ( 'NONE', *, *, #14139, .T. ) ;
#14426 = CARTESIAN_POINT ( 'NONE',  ( -0.2819296736111110424, 0.3513888888130222155, -0.1167790944451423396 ) ) ;
#14427 = CARTESIAN_POINT ( 'NONE',  ( -0.1167790944451424368, 0.08749999992413336203, 0.2819296736111110424 ) ) ;
#14428 = DIRECTION ( 'NONE',  ( -0.000000000000000000, -1.000000000000000000, -0.000000000000000000 ) ) ;
#14429 = FACE_OUTER_BOUND ( 'NONE', #20246, .T. ) ;
#14430 = CARTESIAN_POINT ( 'NONE',  ( 0.2472135954999579166, 0.03214285714285712581, 0.3402603233408160732 ) ) ;
#14431 = CARTESIAN_POINT ( 'NONE',  ( 2.064578755398029967E-15, 5.043833333485014947, -0.3119999999999999996 ) ) ;
#14432 = DIRECTION ( 'NONE',  ( -0.000000000000000000, -1.000000000000000000, -0.000000000000000000 ) ) ;
#14433 = VECTOR ( 'NONE', #6081, 39.37007874015748854 ) ;
#14434 = CARTESIAN_POINT ( 'NONE',  ( -0.1857019731761083148, 3.882747264168788792, -0.2515721468173275910 ) ) ;
#14435 = CARTESIAN_POINT ( 'NONE',  ( 0.000000000000000000, 2.735000000000000320, 0.000000000000000000 ) ) ;
#14436 = CIRCLE ( 'NONE', #7034, 0.01874999999999999237 ) ;
#14437 = CARTESIAN_POINT ( 'NONE',  ( -0.2819296736111110979, 4.422305555631421470, 0.000000000000000000 ) ) ;
#14438 = CARTESIAN_POINT ( 'NONE',  ( 0.000000000000000000, 3.700000000000000622, 0.000000000000000000 ) ) ;
#14439 = CARTESIAN_POINT ( 'NONE',  ( 0.2122370167333460234, 4.522644990543859045, 0.2293254978506919506 ) ) ;
#14440 = CARTESIAN_POINT ( 'NONE',  ( -0.2819296736111110424, 5.029944444520310753, -0.1167790944451423119 ) ) ;
#14441 = LINE ( 'NONE', #21221, #574 ) ;
#14442 = DIRECTION ( 'NONE',  ( 0.000000000000000000, 0.000000000000000000, -1.000000000000000000 ) ) ;
#14443 = CARTESIAN_POINT ( 'NONE',  ( -0.4607735603406451497, -0.2757708160732098568, 0.04763592618481097413 ) ) ;
#14444 = ORIENTED_EDGE ( 'NONE', *, *, #2178, .F. ) ;
#14445 = CARTESIAN_POINT ( 'NONE',  ( -0.1236067977499789583, 0.1982142855192008668, -0.3804226065180614791 ) ) ;
#14446 = CARTESIAN_POINT ( 'NONE',  ( 0.1292346314604058410, 4.408416666818399499, 0.3119999999999998885 ) ) ;
#14447 = CARTESIAN_POINT ( 'NONE',  ( 0.1993543840281266633, 4.512583333409199149, -0.1993543840281266910 ) ) ;
#14448 = CARTESIAN_POINT ( 'NONE',  ( -0.2819296736111110979, 3.908416666742532630, 0.000000000000000000 ) ) ;
#14449 = EDGE_LOOP ( 'NONE', ( #9026, #7303, #10826, #18490 ) ) ;
#14450 = AXIS2_PLACEMENT_3D ( 'NONE', #2429, #9994, #17298 ) ;
#14451 = AXIS2_PLACEMENT_3D ( 'NONE', #20464, #7421, #3761 ) ;
#14452 = ORIENTED_EDGE ( 'NONE', *, *, #17932, .T. ) ;
#14453 = EDGE_CURVE ( 'NONE', #4326, #11465, #14978, .T. ) ;
#14454 = SECURITY_CLASSIFICATION_LEVEL ( 'unclassified' ) ;
#14455 = EDGE_CURVE ( 'NONE', #5544, #7946, #9111, .T. ) ;
#14456 = CARTESIAN_POINT ( 'NONE',  ( -0.1914089481446534236, 4.954695441720193827, 0.2497358724762595572 ) ) ;
#14457 = FACE_OUTER_BOUND ( 'NONE', #2716, .T. ) ;
#14458 = VERTEX_POINT ( 'NONE', #22280 ) ;
#14459 = CARTESIAN_POINT ( 'NONE',  ( 0.1292346314604057023, 0.3340277776260448528, 0.3119999999999998885 ) ) ;
#14460 = CARTESIAN_POINT ( 'NONE',  ( 1.573500000000000343, 2.740000000000000213, -1.412500000000000089 ) ) ;
#14461 = CARTESIAN_POINT ( 'NONE',  ( -0.07998601114778688959, 5.127656800766811074, 0.2972660808172664093 ) ) ;
#14462 = CARTESIAN_POINT ( 'NONE',  ( -0.2209708691207961373, -0.2209708691207961095, -0.09916666666666647256 ) ) ;
#14463 = CARTESIAN_POINT ( 'NONE',  ( 0.1293617830085710407, 0.5441123095027139422, -0.7388485444064273322 ) ) ;
#14464 = ORIENTED_EDGE ( 'NONE', *, *, #19419, .F. ) ;
#14465 = FACE_OUTER_BOUND ( 'NONE', #21585, .T. ) ;
#14466 = CARTESIAN_POINT ( 'NONE',  ( 0.2819296736111110424, 0.3097222221463555303, 0.1167790944451424923 ) ) ;
#14467 = CARTESIAN_POINT ( 'NONE',  ( -0.1954553509668046918, -0.1954553509668046640, 0.3730555555555596925 ) ) ;
#14468 = CARTESIAN_POINT ( 'NONE',  ( -0.1993543840281266355, 4.415361111186976828, 0.1993543840281267465 ) ) ;
#14469 = DIRECTION ( 'NONE',  ( -0.000000000000000000, -1.000000000000000000, -0.000000000000000000 ) ) ;
#14470 = CARTESIAN_POINT ( 'NONE',  ( 0.3003475124358450099, 4.111524471938507119, -3.730379552481990491 ) ) ;
#14471 = CARTESIAN_POINT ( 'NONE',  ( -5.731347020009612645E-17, 0.3861111109593781676, 0.3119999999999999996 ) ) ;
#14472 = CARTESIAN_POINT ( 'NONE',  ( 0.3119999999999999996, 4.134111111111110404, -3.820898013339742174E-17 ) ) ;
#14473 = AXIS2_PLACEMENT_3D ( 'NONE', #14460, #14091, #1163 ) ;
#14474 = CARTESIAN_POINT ( 'NONE',  ( 0.3119999999999999996, 4.974388889040620931, -3.820898013339742174E-17 ) ) ;
#14475 = CARTESIAN_POINT ( 'NONE',  ( 0.2206173157302027954, 4.863277777777777366, -0.2206173157302028232 ) ) ;
#14476 = ORIENTED_EDGE ( 'NONE', *, *, #8866, .T. ) ;
#14477 = PRODUCT_DEFINITION ( 'UNKNOWN', '', #11902, #4601 ) ;
#14478 = CARTESIAN_POINT ( 'NONE',  ( 0.4872114317030045716, 0.000000000000000000, -1.140285115251740145 ) ) ;
#14479 = CARTESIAN_POINT ( 'NONE',  ( 0.1306872919485614071, -0.3155070326520293955, 0.1942361111111139960 ) ) ;
#14480 = CARTESIAN_POINT ( 'NONE',  ( -0.3613381517857144343, 0.4080357141881717498, 0.1174058825155740171 ) ) ;
#14481 = CARTESIAN_POINT ( 'NONE',  ( 0.2727340197566651137, -0.3838028176415952397, 0.4171892680188027391 ) ) ;
#14482 = CARTESIAN_POINT ( 'NONE',  ( 0.1116596296178199027, 0.1937499999024575870, 0.3436530038418508792 ) ) ;
#14483 = CARTESIAN_POINT ( 'NONE',  ( -0.1993543840281267465, 0.3618055554796889006, 0.1993543840281266633 ) ) ;
#14484 = CARTESIAN_POINT ( 'NONE',  ( 0.000000000000000000, 0.2764156081756484196, 0.2480555555555586933 ) ) ;
#14485 = CARTESIAN_POINT ( 'NONE',  ( -0.2819296736111110424, 5.252166666742532186, -0.1167790944451423119 ) ) ;
#14486 = CARTESIAN_POINT ( 'NONE',  ( 1.573500000000000343, 0.000000000000000000, -1.818749999999999867 ) ) ;
#14487 = VERTEX_POINT ( 'NONE', #5576 ) ;
#14488 = CARTESIAN_POINT ( 'NONE',  ( 5.731347020009612645E-17, 3.842444444444443441, 0.3119999999999999996 ) ) ;
#14489 = EDGE_CURVE ( 'NONE', #22355, #20229, #23852, .T. ) ;
#14490 = CARTESIAN_POINT ( 'NONE',  ( 0.01770140881492013318, 4.876688247272896071, -0.3115197202295738044 ) ) ;
#14491 = CARTESIAN_POINT ( 'NONE',  ( 2.159030003005114828, 2.291712385858714285, -2.568740473580834127 ) ) ;
#14492 = DIRECTION ( 'NONE',  ( 0.000000000000000000, -1.000000000000000000, 1.493785812010397437E-17 ) ) ;
#14493 = CARTESIAN_POINT ( 'NONE',  ( 0.1292346314604058410, 4.679249999999998799, 0.3119999999999998885 ) ) ;
#14494 = CARTESIAN_POINT ( 'NONE',  ( 0.06933867596744393291, 5.200618429028261325, 0.2766904312229080953 ) ) ;
#14495 = EDGE_CURVE ( 'NONE', #12271, #12827, #10837, .T. ) ;
#14496 = CARTESIAN_POINT ( 'NONE',  ( -0.1167790944451423535, 3.918833333409198705, 0.2819296736111110979 ) ) ;
#14497 = CARTESIAN_POINT ( 'NONE',  ( -0.2819296736111110424, 3.752166666742533074, -0.1167790944451423119 ) ) ;
#14498 = CARTESIAN_POINT ( 'NONE',  ( 0.06970122686329188744, 4.041909198427281247, -0.3046041375326968281 ) ) ;
#14499 = CARTESIAN_POINT ( 'NONE',  ( 0.01848103877826402786, 0.5441716683897283025, 0.04413116910602140480 ) ) ;
#14500 = ORIENTED_EDGE ( 'NONE', *, *, #940, .F. ) ;
#14501 = CARTESIAN_POINT ( 'NONE',  ( -0.3119999999999999996, 4.550777777777777366, 0.000000000000000000 ) ) ;
#14502 = CARTESIAN_POINT ( 'NONE',  ( -0.2819296736111110424, 4.467444444520308977, 0.1167790944451424923 ) ) ;
#14503 = EDGE_CURVE ( 'NONE', #9355, #20185, #406, .T. ) ;
#14504 = CARTESIAN_POINT ( 'NONE',  ( -0.3118796326775569172, 4.502940687055745350, 0.02682079161860434491 ) ) ;
#14505 = VECTOR ( 'NONE', #6904, 39.37007874015748143 ) ;
#14506 = PERSON_AND_ORGANIZATION ( #15518, #2538 ) ;
#14507 = CARTESIAN_POINT ( 'NONE',  ( -0.1961415469429297342, -0.1956144934194087859, -0.06558227484231513027 ) ) ;
#14508 = CARTESIAN_POINT ( 'NONE',  ( -0.1144950937579609918, -0.2764156081756484196, 0.3209722222222259891 ) ) ;
#14509 = CARTESIAN_POINT ( 'NONE',  ( -0.2819296736111110979, 3.811194444520310309, 0.000000000000000000 ) ) ;
#14510 = CARTESIAN_POINT ( 'NONE',  ( -0.4316174467094646694, 1.999640111863030256, -2.863205824962447021 ) ) ;
#14511 = DIRECTION ( 'NONE',  ( 0.000000000000000000, 0.000000000000000000, -1.000000000000000000 ) ) ;
#14512 = CARTESIAN_POINT ( 'NONE',  ( 0.3119999999999999996, 0.07013888873715595773, -0.1292346314604056468 ) ) ;
#14513 = CARTESIAN_POINT ( 'NONE',  ( -0.2233192592356399442, -0.03482142866897096345, -0.3073725909049500049 ) ) ;
#14514 = CARTESIAN_POINT ( 'NONE',  ( -0.1993543840281267465, 0.3479166665908000611, 0.1993543840281266633 ) ) ;
#14515 = CARTESIAN_POINT ( 'NONE',  ( -0.08187103065728323914, 0.2793464338139786673, 0.4021514253947122142 ) ) ;
#14516 = LINE ( 'NONE', #12576, #10802 ) ;
#14517 = CARTESIAN_POINT ( 'NONE',  ( -0.1669947351848384554, 0.5031321662965324570, -0.7312129885460184608 ) ) ;
#14518 = CARTESIAN_POINT ( 'NONE',  ( -3.385114897866767815E-17, -0.2764156081756484196, -0.008888888888887782128 ) ) ;
#14519 = CARTESIAN_POINT ( 'NONE',  ( -0.1144950937579609918, -0.2764156081756484196, 0.05013888888889045381 ) ) ;
#14520 = ORIENTED_EDGE ( 'NONE', *, *, #14324, .T. ) ;
#14521 = VERTEX_POINT ( 'NONE', #11196 ) ;
#14522 = CARTESIAN_POINT ( 'NONE',  ( 4.113055369932088708E-16, 0.09642857142857140518, 0.4000000000000000222 ) ) ;
#14523 = CARTESIAN_POINT ( 'NONE',  ( -0.3038794317022511793, 3.833275345265239942, -0.08166550760139516807 ) ) ;
#14524 = CARTESIAN_POINT ( 'NONE',  ( 0.3119999999999998885, 0.1256944444444441089, 0.1292346314604058410 ) ) ;
#14525 = ADVANCED_FACE ( 'NONE', ( #5458 ), #12924, .F. ) ;
#14526 = CARTESIAN_POINT ( 'NONE',  ( 0.2819296736111110424, 3.953555555631421914, -0.1167790944451423396 ) ) ;
#14527 = CARTESIAN_POINT ( 'NONE',  ( 2.326421213736078119E-17, 0.2437499999024574926, -0.3799334167787516425 ) ) ;
#14528 = AXIS2_PLACEMENT_3D ( 'NONE', #13338, #9426, #4051 ) ;
#14529 = CARTESIAN_POINT ( 'NONE',  ( -0.1167790944451423535, 4.488277777853644679, 0.2819296736111110424 ) ) ;
#14530 = CARTESIAN_POINT ( 'NONE',  ( 0.000000000000000000, 0.02999999999999995379, 0.000000000000000000 ) ) ;
#14531 = CARTESIAN_POINT ( 'NONE',  ( 5.731347020009612645E-17, 4.397999999999999687, 0.3119999999999999996 ) ) ;
#14532 = ORIENTED_EDGE ( 'NONE', *, *, #17117, .F. ) ;
#14533 = CARTESIAN_POINT ( 'NONE',  ( 0.2472135954999579166, 0.3892857142857142350, 0.3402603233408160732 ) ) ;
#14534 = CARTESIAN_POINT ( 'NONE',  ( 0.2819296736111110979, 5.154944444520308977, 0.1167790944451422425 ) ) ;
#14535 = EDGE_CURVE ( 'NONE', #20593, #20299, #23349, .T. ) ;
#14536 = CARTESIAN_POINT ( 'NONE',  ( 0.02226199859978414408, 4.209868373251637763, -0.3112347022699947230 ) ) ;
#14537 = CARTESIAN_POINT ( 'NONE',  ( 0.3999999999999999667, 0.2446428569477722970, 0.1299678784931626307 ) ) ;
#14538 = CARTESIAN_POINT ( 'NONE',  ( -5.731347020009612645E-17, 0.2263888888888885564, 0.3119999999999999996 ) ) ;
#14539 = CARTESIAN_POINT ( 'NONE',  ( -0.1167790944451423535, 4.863277777853642903, 0.2819296736111110979 ) ) ;
#14540 = PERSON_AND_ORGANIZATION ( #9732, #14658 ) ;
#14541 = CARTESIAN_POINT ( 'NONE',  ( -0.1618391056162997999, 4.066759731312079573, 0.2668031243805282782 ) ) ;
#14542 = EDGE_CURVE ( 'NONE', #13117, #16849, #86, .T. ) ;
#14543 = CARTESIAN_POINT ( 'NONE',  ( -0.2206173157302027954, 0.4208333331816004330, -0.2206173157302028232 ) ) ;
#14544 = EDGE_LOOP ( 'NONE', ( #6289, #8734, #23519, #19100, #9951 ) ) ;
#14545 = CARTESIAN_POINT ( 'NONE',  ( 0.1993543840281266355, 0.2090277777019111383, 0.1993543840281267465 ) ) ;
#14546 = ORIENTED_EDGE ( 'NONE', *, *, #10189, .F. ) ;
#14547 = CARTESIAN_POINT ( 'NONE',  ( 1.726321361862525858E-17, 0.06319444436857780956, -0.2819296736111110979 ) ) ;
#14548 = CARTESIAN_POINT ( 'NONE',  ( -1.546911548986461295E-15, 2.740000000000000213, -2.515999999999997794 ) ) ;
#14549 = DIRECTION ( 'NONE',  ( 0.8320502943378439431, -0.4803844614152621428, 0.2773500981126125753 ) ) ;
#14550 = CARTESIAN_POINT ( 'NONE',  ( -0.4000000000000000222, 0.007142857142857113144, -4.898587196589413075E-17 ) ) ;
#14551 = CARTESIAN_POINT ( 'NONE',  ( -0.3119999999999998885, 3.776472222222221564, 0.1292346314604058410 ) ) ;
#14552 = EDGE_CURVE ( 'NONE', #23019, #10368, #8860, .T. ) ;
#14553 = CARTESIAN_POINT ( 'NONE',  ( -0.2517964863178585588, 3.885433942164395305, -0.1842776042936377368 ) ) ;
#14554 = CARTESIAN_POINT ( 'NONE',  ( 0.1993543840281266910, -0.01319444452031107509, -0.1993543840281266910 ) ) ;
#14555 = EDGE_CURVE ( 'NONE', #10744, #9500, #22523, .T. ) ;
#14556 = CARTESIAN_POINT ( 'NONE',  ( 0.2819296736111110424, 4.620222222298088433, -0.1167790944451423396 ) ) ;
#14557 = FACE_OUTER_BOUND ( 'NONE', #18695, .T. ) ;
#14558 = CARTESIAN_POINT ( 'NONE',  ( 0.2060069779502269882, 4.537481089443112126, -0.2362988211741367806 ) ) ;
#14559 = CARTESIAN_POINT ( 'NONE',  ( 5.178964085587577574E-17, 4.991750000075866112, 0.2819296736111110979 ) ) ;
#14560 = CARTESIAN_POINT ( 'NONE',  ( -0.2993415042824079109, 0.05277108377353196406, 0.04638604691508683292 ) ) ;
#14561 = CARTESIAN_POINT ( 'NONE',  ( 0.07147791734704542210, 3.764038038968208877, -0.3039139294749904074 ) ) ;
#14562 = CARTESIAN_POINT ( 'NONE',  ( -0.09435543239135868454, 3.514980167629567998, 2.763260016782451700 ) ) ;
#14563 = CARTESIAN_POINT ( 'NONE',  ( -0.4620259694561524855, 0.2880908832651557505, 0.04413116910601658227 ) ) ;
#14564 = CARTESIAN_POINT ( 'NONE',  ( -1.910449006669871087E-17, 4.266055555707287894, -0.3119999999999999996 ) ) ;
#14565 = CIRCLE ( 'NONE', #18064, 0.2500000000000000000 ) ;
#14566 = EDGE_CURVE ( 'NONE', #5262, #19113, #7883, .T. ) ;
#14567 = CARTESIAN_POINT ( 'NONE',  ( -1.726321361862525858E-17, 4.519527777853643791, -0.2819296736111110979 ) ) ;
#14568 = CARTESIAN_POINT ( 'NONE',  ( -0.1167790944451423535, 3.863277777853643791, 0.2819296736111110424 ) ) ;
#14569 = VERTEX_POINT ( 'NONE', #9483 ) ;
#14570 = VERTEX_POINT ( 'NONE', #22763 ) ;
#14571 = PERSON_AND_ORGANIZATION ( #15518, #2538 ) ;
#14572 = CYLINDRICAL_SURFACE ( 'NONE', #9211, 0.3119999999999999996 ) ;
#14573 = ADVANCED_FACE ( 'NONE', ( #16915 ), #569, .T. ) ;
#14574 = CARTESIAN_POINT ( 'NONE',  ( -0.1572786115130385687, 4.937427088230124106, -0.2725414607716101223 ) ) ;
#14575 = PLANE ( 'NONE',  #4220 ) ;
#14576 = ORIENTED_EDGE ( 'NONE', *, *, #16946, .F. ) ;
#14577 = CARTESIAN_POINT ( 'NONE',  ( 1.910449006669871087E-17, 0.2472222220704892726, -0.3119999999999999996 ) ) ;
#14578 = CARTESIAN_POINT ( 'NONE',  ( -0.2476943800122561878, 4.396861609578765595, 0.1908053648353139065 ) ) ;
#14579 = DIRECTION ( 'NONE',  ( 0.000000000000000000, 1.000000000000000000, 0.000000000000000000 ) ) ;
#14580 = AXIS2_PLACEMENT_3D ( 'NONE', #19604, #8505, #15945 ) ;
#14581 = LINE ( 'NONE', #20421, #20470 ) ;
#14582 = CARTESIAN_POINT ( 'NONE',  ( 0.2019315168632336566, 0.3017797859643823188, -0.7223231963670132538 ) ) ;
#14583 = VERTEX_POINT ( 'NONE', #15099 ) ;
#14584 = ORIENTED_EDGE ( 'NONE', *, *, #7642, .T. ) ;
#14585 = ORIENTED_EDGE ( 'NONE', *, *, #13236, .F. ) ;
#14586 = CARTESIAN_POINT ( 'NONE',  ( 0.1989253662351168350, 5.077772732731912875, 0.2405052583373312181 ) ) ;
#14587 = CARTESIAN_POINT ( 'NONE',  ( -3.385114897866767815E-17, -0.2764156081756484196, 0.3244444444444482545 ) ) ;
#14588 = CARTESIAN_POINT ( 'NONE',  ( -1.726321361862525858E-17, 4.116750000075865223, -0.2819296736111110979 ) ) ;
#14589 = CARTESIAN_POINT ( 'NONE',  ( 0.1167790944451424506, 5.092444444520309865, 0.2819296736111110424 ) ) ;
#14590 = CARTESIAN_POINT ( 'NONE',  ( -0.1312453311288143964, -0.4543582620183869158, 0.4268234664230690090 ) ) ;
#14591 = DIRECTION ( 'NONE',  ( 1.000000000000000000, 0.000000000000000000, -0.000000000000000000 ) ) ;
#14592 = CARTESIAN_POINT ( 'NONE',  ( -0.1292346314604056745, 3.984805555555554601, -0.3119999999999999996 ) ) ;
#14593 = EDGE_CURVE ( 'NONE', #19970, #17585, #6344, .T. ) ;
#14594 = CARTESIAN_POINT ( 'NONE',  ( -0.1292346314604057023, 4.957027777929510215, 0.3119999999999998885 ) ) ;
#14595 = EDGE_CURVE ( 'NONE', #24062, #544, #13280, .T. ) ;
#14596 = CARTESIAN_POINT ( 'NONE',  ( 5.178964085587577574E-17, 5.158416666742532186, 0.2819296736111110979 ) ) ;
#14597 = CARTESIAN_POINT ( 'NONE',  ( 0.3119999999999999996, 4.859805555555554157, -0.1292346314604056745 ) ) ;
#14598 = ORIENTED_EDGE ( 'NONE', *, *, #18638, .T. ) ;
#14599 = AXIS2_PLACEMENT_3D ( 'NONE', #21665, #18011, #6912 ) ;
#14600 = CARTESIAN_POINT ( 'NONE',  ( -0.1331525752728061063, 0.05822810958904708900, 0.2781245439472574410 ) ) ;
#14601 = CARTESIAN_POINT ( 'NONE',  ( 0.000000000000000000, 0.3155070326520292845, 0.2740972222222257670 ) ) ;
#14602 = CARTESIAN_POINT ( 'NONE',  ( 0.2923287055106771337, 0.3758928570453146656, -0.2123892367102620249 ) ) ;
#14603 = CARTESIAN_POINT ( 'NONE',  ( 0.3880456933851195167, -0.3172275918314949039, 0.4112725064128996966 ) ) ;
#14604 = PRODUCT_DEFINITION_SHAPE ( 'NONE', 'NONE',  #13174 ) ;
#14605 = CARTESIAN_POINT ( 'NONE',  ( 3.061616997868383634E-17, 5.580000000000000959, -0.2500000000000000555 ) ) ;
#14606 = B_SPLINE_CURVE_WITH_KNOTS ( 'NONE', 3,
 ( #13524, #11319, #7653, #13396, #4108, #11568 ),
 .UNSPECIFIED., .F., .F.,
 ( 4, 2, 4 ),
 ( 0.000000000000000000, 0.0002551367231383061714, 0.0005102734462766123427 ),
 .UNSPECIFIED. ) ;
#14607 = CARTESIAN_POINT ( 'NONE',  ( 1.726321361862525858E-17, 0.3409722221463556413, -0.2819296736111110979 ) ) ;
#14608 = CARTESIAN_POINT ( 'NONE',  ( -0.2764156081756484196, 0.1144950937579609918, 0.2584722222222254340 ) ) ;
#14609 = CARTESIAN_POINT ( 'NONE',  ( 0.1167790944451424368, 5.106333333409198261, 0.2819296736111110424 ) ) ;
#14610 = CARTESIAN_POINT ( 'NONE',  ( -0.4795759075923621273, -5.504308098328212156E-13, 0.07439896364136201756 ) ) ;
#14611 = VECTOR ( 'NONE', #13179, 39.37007874015748854 ) ;
#14612 = CARTESIAN_POINT ( 'NONE',  ( 0.1993543840281266633, 4.998694444520309865, -0.1993543840281266910 ) ) ;
#14613 = CARTESIAN_POINT ( 'NONE',  ( -0.4000000000000000222, 0.06964285694777233582, -4.898587196589413075E-17 ) ) ;
#14614 = CARTESIAN_POINT ( 'NONE',  ( 0.0001028783557116418908, 4.877163902639057191, -0.3119999876241853487 ) ) ;
#14615 = CARTESIAN_POINT ( 'NONE',  ( 0.3120000000000000551, 4.575083333333332725, 0.1292346314604056190 ) ) ;
#14616 = DIRECTION ( 'NONE',  ( -0.000000000000000000, -1.000000000000000000, -0.000000000000000000 ) ) ;
#14617 = CARTESIAN_POINT ( 'NONE',  ( -0.3119999999999999996, 4.661888888888888083, 0.000000000000000000 ) ) ;
#14618 = CARTESIAN_POINT ( 'NONE',  ( 0.1167790944451422702, 4.113277777853642903, -0.2819296736111110979 ) ) ;
#14619 = CARTESIAN_POINT ( 'NONE',  ( -0.1993543840281266910, 3.748694444520310309, -0.1993543840281266910 ) ) ;
#14620 =( BOUNDED_SURFACE ( )  B_SPLINE_SURFACE ( 3, 2, ( 
 ( #18680, #16856, #142 ),
 ( #3929, #7585, #7705 ),
 ( #22459, #5758, #2228 ),
 ( #13329, #9537, #15270 ),
 ( #13452, #13219, #11373 ),
 ( #4164, #7348, #16970 ),
 ( #11614, #9175, #14800 ),
 ( #4042, #11495, #22215 ),
 ( #18930, #5515, #12978 ),
 ( #20395, #3686, #18561 ) ),
 .UNSPECIFIED., .F., .F., .T. ) 
 B_SPLINE_SURFACE_WITH_KNOTS ( ( 4, 2, 2, 2, 4 ),
 ( 3, 3 ),
 ( 0.04463809143445898742, 0.04796255359614957914, 0.05128701575784017780, 0.05461147791953077646, 0.05793594008122136818 ),
 ( 0.000000000000000000, 1.000000000000000000 ),
 .UNSPECIFIED. ) 
 GEOMETRIC_REPRESENTATION_ITEM ( )  RATIONAL_B_SPLINE_SURFACE ( (
 ( 1.000000000000000000, 0.8285407536241353732, 1.000000000000000000),
 ( 1.000000000000000000, 0.8326168960428802501, 1.000000000000000000),
 ( 1.000000000000000000, 0.8363786027323344419, 1.000000000000000000),
 ( 1.000000000000000000, 0.8417912930207894773, 1.000000000000000000),
 ( 1.000000000000000000, 0.8433923807920618021, 1.000000000000000000),
 ( 1.000000000000000000, 0.8433905099813472361, 1.000000000000000000),
 ( 1.000000000000000000, 0.8417888685871616206, 1.000000000000000000),
 ( 1.000000000000000000, 0.8363766775000033293, 1.000000000000000000),
 ( 1.000000000000000000, 0.8326159398062557004, 1.000000000000000000),
 ( 1.000000000000000000, 0.8285407536241354842, 1.000000000000000000) ) ) 
 REPRESENTATION_ITEM ( '' )  SURFACE ( )  );
#14621 = CARTESIAN_POINT ( 'NONE',  ( 0.2877648753177015628, 4.033457023929424956, -0.1207660770027009639 ) ) ;
#14622 = CARTESIAN_POINT ( 'NONE',  ( -5.731347020009612645E-17, 0.3930555555555551583, 0.3119999999999999996 ) ) ;
#14623 = APPROVAL_PERSON_ORGANIZATION ( #22507, #9095, #11781 ) ;
#14624 = VERTEX_POINT ( 'NONE', #19702 ) ;
#14625 = DIRECTION ( 'NONE',  ( -0.8660254037844420383, 0.000000000000000000, 0.4999999999999942268 ) ) ;
#14626 = ORIENTED_EDGE ( 'NONE', *, *, #16172, .F. ) ;
#14627 = CARTESIAN_POINT ( 'NONE',  ( 5.178964085587577574E-17, 4.255638888964754507, 0.2819296736111110979 ) ) ;
#14628 = CARTESIAN_POINT ( 'NONE',  ( -0.2416764884589730211, 4.508252704873092043, 0.1973253190368417231 ) ) ;
#14629 = VECTOR ( 'NONE', #14701, 39.37007874015748143 ) ;
#14630 = DIRECTION ( 'NONE',  ( -0.000000000000000000, -1.000000000000000000, -0.000000000000000000 ) ) ;
#14631 = CARTESIAN_POINT ( 'NONE',  ( -0.2764156081756484196, 0.1144950937579609918, 0.1404166666666689656 ) ) ;
#14632 = DIRECTION ( 'NONE',  ( -0.000000000000000000, -1.000000000000000000, -0.000000000000000000 ) ) ;
#14633 = CARTESIAN_POINT ( 'NONE',  ( 0.4719654084974829189, 0.2800274776536548771, 0.04212966708837325575 ) ) ;
#14634 = CARTESIAN_POINT ( 'NONE',  ( 0.3104386443325673484, 0.3620340424930042489, 0.08855526556984563702 ) ) ;
#14635 = CYLINDRICAL_SURFACE ( 'NONE', #20589, 0.2500000000000000000 ) ;
#14636 = LOCAL_TIME ( 21, 9, 13.00000000000000000, #16872 ) ;
#14637 = CARTESIAN_POINT ( 'NONE',  ( 0.1116596296178199027, 0.3544642856167432576, 0.3436530038418508792 ) ) ;
#14638 = CARTESIAN_POINT ( 'NONE',  ( 1.726321361862525858E-17, 0.2159722221463555858, -0.2819296736111110979 ) ) ;
#14639 = CARTESIAN_POINT ( 'NONE',  ( 0.3120005064808646922, 3.864374921735875379, -0.04083496376970818104 ) ) ;
#14640 = DIRECTION ( 'NONE',  ( -0.8660254037844394848, 0.4999999999999983902, -0.000000000000000000 ) ) ;
#14641 = PRODUCT_RELATED_PRODUCT_CATEGORY ( 'detail', '', ( #10911 ) ) ;
#14642 = CARTESIAN_POINT ( 'NONE',  ( -0.2055620820422562611, 0.3152427873485467158, -0.7212836743131715300 ) ) ;
#14643 = CARTESIAN_POINT ( 'NONE',  ( -0.1144950937579609779, 0.2764156081756484196, -0.1373611111111110450 ) ) ;
#14644 = ORIENTED_EDGE ( 'NONE', *, *, #23553, .T. ) ;
#14645 = ORIENTED_EDGE ( 'NONE', *, *, #9464, .F. ) ;
#14646 = DIRECTION ( 'NONE',  ( -0.000000000000000000, -1.000000000000000000, -0.000000000000000000 ) ) ;
#14647 = CARTESIAN_POINT ( 'NONE',  ( -0.3119999999999999996, 4.713972222222221120, -0.1292346314604056468 ) ) ;
#14648 = CARTESIAN_POINT ( 'NONE',  ( -0.1292346314604058410, 0.0006944444444441107535, 0.3119999999999998885 ) ) ;
#14649 = CARTESIAN_POINT ( 'NONE',  ( -0.1167790944451423257, 3.856333333409198705, -0.2819296736111110424 ) ) ;
#14650 = CARTESIAN_POINT ( 'NONE',  ( -0.3613381517857143232, 0.2580357141881718386, -0.1174058825155741004 ) ) ;
#14651 = VECTOR ( 'NONE', #22511, 39.37007874015748143 ) ;
#14652 = CARTESIAN_POINT ( 'NONE',  ( 0.1993543840281267465, 4.443138888964754507, 0.1993543840281266633 ) ) ;
#14653 = DIRECTION ( 'NONE',  ( -0.000000000000000000, -1.000000000000000000, -0.000000000000000000 ) ) ;
#14654 = DIRECTION ( 'NONE',  ( 0.000000000000000000, 0.000000000000000000, -1.000000000000000000 ) ) ;
#14655 = EDGE_LOOP ( 'NONE', ( #3309, #10986, #11543, #23991 ) ) ;
#14656 = CARTESIAN_POINT ( 'NONE',  ( 0.05907641261700106311, 4.375511868578897179, -0.3066178703699756758 ) ) ;
#14657 = CARTESIAN_POINT ( 'NONE',  ( 0.1167790944451422702, 5.168833333409199149, -0.2819296736111110424 ) ) ;
#14658 = ORGANIZATION ( 'NAUO-ORG1', 'UNSPECIFIED', 'UNSPECIFIED' ) ;
#14659 = DIRECTION ( 'NONE',  ( 0.000000000000000000, 0.000000000000000000, 1.000000000000000000 ) ) ;
#14660 =( LENGTH_UNIT ( ) NAMED_UNIT ( * ) SI_UNIT ( $, .METRE. ) );
#14661 = DIRECTION ( 'NONE',  ( 0.7745966692414850696, -0.4472135954999565954, 0.4472135954999565954 ) ) ;
#14662 = FACE_OUTER_BOUND ( 'NONE', #4086, .T. ) ;
#14663 = VECTOR ( 'NONE', #20028, 39.37007874015748143 ) ;
#14664 = CARTESIAN_POINT ( 'NONE',  ( 0.1993543840281266633, 4.665361111186976828, -0.1993543840281266910 ) ) ;
#14666 = EDGE_CURVE ( 'NONE', #20003, #11169, #2760, .T. ) ;
#14665 = COORDINATED_UNIVERSAL_TIME_OFFSET ( 0, 0, .AHEAD. ) ;
#14667 = VECTOR ( 'NONE', #4196, 39.37007874015748854 ) ;
#14668 = CARTESIAN_POINT ( 'NONE',  ( -0.4675595609217420567, 0.2849403337939152570, 0.04271891838947983189 ) ) ;
#14669 = CARTESIAN_POINT ( 'NONE',  ( -0.4593750000000004219, -0.2760455974562901482, 0.06112444011295364160 ) ) ;
#14670 = CARTESIAN_POINT ( 'NONE',  ( 0.1167790944451423257, 0.6152777777019110550, -0.2819296736111110424 ) ) ;
#14671 = VERTEX_POINT ( 'NONE', #23106 ) ;
#14672 = ORIENTED_EDGE ( 'NONE', *, *, #19643, .F. ) ;
#14673 = CARTESIAN_POINT ( 'NONE',  ( 0.1167790944451423257, 0.2819444443685777957, -0.2819296736111110424 ) ) ;
#14674 = FACE_OUTER_BOUND ( 'NONE', #12155, .T. ) ;
#14675 = CARTESIAN_POINT ( 'NONE',  ( -0.3566234456863465740, 3.685658299244018998, 2.638859501304836375 ) ) ;
#14676 = CARTESIAN_POINT ( 'NONE',  ( 0.4000000000000000222, 0.04285714285714282978, 0.000000000000000000 ) ) ;
#14677 = CARTESIAN_POINT ( 'NONE',  ( 0.1306872919485616846, 0.3155070326520292290, -0.01062499999999911779 ) ) ;
#14678 = EDGE_CURVE ( 'NONE', #9027, #7279, #5075, .T. ) ;
#14679 = DIRECTION ( 'NONE',  ( 0.000000000000000000, -0.2142211582677940040, 0.9767851838303059919 ) ) ;
#14680 = CARTESIAN_POINT ( 'NONE',  ( 3.820898013339742174E-17, 5.384999999999999787, 0.3119999999999999996 ) ) ;
#14681 = CARTESIAN_POINT ( 'NONE',  ( -0.1167790944451423257, 4.467444444520309865, -0.2819296736111110424 ) ) ;
#14682 = CARTESIAN_POINT ( 'NONE',  ( -0.1993543840281267465, 0.01458333325746670114, 0.1993543840281266633 ) ) ;
#14683 = CARTESIAN_POINT ( 'NONE',  ( -0.2819296736111110424, 4.585500000075865223, -0.1167790944451423119 ) ) ;
#14684 = CARTESIAN_POINT ( 'NONE',  ( -0.4000000000000000222, 0.07321428551920092231, 0.1299678784931624920 ) ) ;
#14685 = CARTESIAN_POINT ( 'NONE',  ( 0.02106394849456709809, 4.543234972684153661, -0.3113162720545575857 ) ) ;
#14686 = CARTESIAN_POINT ( 'NONE',  ( -0.1167790944451423257, 5.023000000075867000, -0.2819296736111110424 ) ) ;
#14687 = CARTESIAN_POINT ( 'NONE',  ( 0.1993543840281266633, 4.443138888964754507, -0.1993543840281266910 ) ) ;
#14688 = CARTESIAN_POINT ( 'NONE',  ( 0.2902266206095440726, 3.748848065998740875, 0.1156229089065601984 ) ) ;
#14689 = CARTESIAN_POINT ( 'NONE',  ( -0.3120000000000000551, 0.4868055554038225874, 0.1292346314604056190 ) ) ;
#14690 = VECTOR ( 'NONE', #22783, 39.37007874015748143 ) ;
#14691 = CARTESIAN_POINT ( 'NONE',  ( -3.345742422185251127E-06, 4.766055647721512578, -0.3119999999820609049 ) ) ;
#14692 = CARTESIAN_POINT ( 'NONE',  ( -0.3119999999999999996, 4.220916666818398610, -0.1292346314604056468 ) ) ;
#14693 = CARTESIAN_POINT ( 'NONE',  ( -0.1993543840281266355, 4.484805555631421470, 0.1993543840281267465 ) ) ;
#14694 = CARTESIAN_POINT ( 'NONE',  ( 0.1993543840281266633, 3.832027777853643791, -0.1993543840281266910 ) ) ;
#14695 = ORIENTED_EDGE ( 'NONE', *, *, #21858, .F. ) ;
#14696 = EDGE_CURVE ( 'NONE', #18852, #11248, #15261, .T. ) ;
#14697 = ADVANCED_FACE ( 'NONE', ( #15287 ), #3930, .T. ) ;
#14698 = VERTEX_POINT ( 'NONE', #520 ) ;
#14699 = APPROVAL_ROLE ( '' ) ;
#14700 = DIRECTION ( 'NONE',  ( -0.4999999999999913403, 0.000000000000000000, 0.8660254037844437036 ) ) ;
#14701 = DIRECTION ( 'NONE',  ( 0.000000000000000000, 0.000000000000000000, 1.000000000000000000 ) ) ;
#14702 = FACE_OUTER_BOUND ( 'NONE', #5851, .T. ) ;
#14703 = VERTEX_POINT ( 'NONE', #22838 ) ;
#14704 = CARTESIAN_POINT ( 'NONE',  ( 0.3119999999999999996, 0.2333333331816004053, 0.000000000000000000 ) ) ;
#14705 = VECTOR ( 'NONE', #8141, 39.37007874015748854 ) ;
#14706 = CARTESIAN_POINT ( 'NONE',  ( -2.750539236387841874E-07, 4.266055563097283176, -0.3119999999998787632 ) ) ;
#14707 = CARTESIAN_POINT ( 'NONE',  ( 5.731347020009612645E-17, 4.509111111111110404, 0.3119999999999999996 ) ) ;
#14708 = CARTESIAN_POINT ( 'NONE',  ( 0.000000000000000000, 0.9300000000000000488, 0.000000000000000000 ) ) ;
#14709 = DIRECTION ( 'NONE',  ( 0.000000000000000000, 0.000000000000000000, 1.000000000000000000 ) ) ;
#14710 = ADVANCED_FACE ( 'NONE', ( #11757 ), #19105, .F. ) ;
#14711 = ORIENTED_EDGE ( 'NONE', *, *, #1288, .T. ) ;
#14712 = CARTESIAN_POINT ( 'NONE',  ( -0.1116596296178200276, 0.06160714275960046254, 0.3436530038418508792 ) ) ;
#14713 = ORIENTED_EDGE ( 'NONE', *, *, #11728, .F. ) ;
#14714 = LINE ( 'NONE', #16288, #23961 ) ;
#14715 = CARTESIAN_POINT ( 'NONE',  ( 0.2764156081756484196, -5.077672346800151106E-17, 0.3383333333333372051 ) ) ;
#14716 = CARTESIAN_POINT ( 'NONE',  ( 0.1167790944451422702, 4.224388888964755395, -0.2819296736111110424 ) ) ;
#14717 = CARTESIAN_POINT ( 'NONE',  ( 0.1167790944451422702, 5.113277777853642903, -0.2819296736111110979 ) ) ;
#14718 = CARTESIAN_POINT ( 'NONE',  ( -0.4687500000000003886, 0.2598076211353315124, 0.06112444011295379426 ) ) ;
#14719 = CARTESIAN_POINT ( 'NONE',  ( -0.3036138212764256661, 4.226459472032660258, 0.07378917105941848464 ) ) ;
#14720 = PLANE ( 'NONE',  #13682 ) ;
#14721 = CARTESIAN_POINT ( 'NONE',  ( 0.3119999999999999996, 4.922305555707287006, -0.1292346314604056745 ) ) ;
#14722 = CARTESIAN_POINT ( 'NONE',  ( -0.2082794372640225100, 5.206640035683668621, 0.1900105704308308607 ) ) ;
#14723 = EDGE_CURVE ( 'NONE', #20411, #2118, #7905, .T. ) ;
#14724 = AXIS2_PLACEMENT_3D ( 'NONE', #6905, #14343, #21776 ) ;
#14725 = CARTESIAN_POINT ( 'NONE',  ( -0.2977100099089716734, 3.659999999999999698, 0.09499999999999995948 ) ) ;
#14726 = ORIENTED_EDGE ( 'NONE', *, *, #8866, .F. ) ;
#14727 = CARTESIAN_POINT ( 'NONE',  ( 0.2562433651785209210, -0.1785792061920698504, 0.4235489577189899268 ) ) ;
#14728 = CARTESIAN_POINT ( 'NONE',  ( -0.2194851440959312838, 0.05625703873743409522, 0.2130962475854012161 ) ) ;
#14729 = ORIENTED_EDGE ( 'NONE', *, *, #12728, .T. ) ;
#14730 = CARTESIAN_POINT ( 'NONE',  ( 0.3155070326520292290, 0.1306872919485615736, 0.2636805555555590264 ) ) ;
#14731 = CARTESIAN_POINT ( 'NONE',  ( -0.1167790944451423257, 5.009111111186976828, -0.2819296736111110424 ) ) ;
#14732 = CARTESIAN_POINT ( 'NONE',  ( 0.4228029066818827508, -0.2971605053783332728, 0.3901413544831415781 ) ) ;
#14733 = EDGE_CURVE ( 'NONE', #19306, #4696, #19299, .T. ) ;
#14734 = CARTESIAN_POINT ( 'NONE',  ( 0.1116596296178199860, 0.3651785713310289894, -0.3436530038418508792 ) ) ;
#14735 = AXIS2_PLACEMENT_3D ( 'NONE', #15223, #13529, #2415 ) ;
#14736 = ORIENTED_EDGE ( 'NONE', *, *, #13236, .T. ) ;
#14737 = CARTESIAN_POINT ( 'NONE',  ( -5.178964085587577574E-17, 0.3131944443685777957, 0.2819296736111110979 ) ) ;
#14738 = CARTESIAN_POINT ( 'NONE',  ( 0.2764156081756483641, 0.1144950937579610056, 0.2931944444444479214 ) ) ;
#14739 = CARTESIAN_POINT ( 'NONE',  ( 0.1167790944451424368, 4.939666666742532186, 0.2819296736111110424 ) ) ;
#14740 = CARTESIAN_POINT ( 'NONE',  ( 0.01010037888641339247, 4.487987261627375268, -0.3119999999597998785 ) ) ;
#14741 = ORIENTED_EDGE ( 'NONE', *, *, #10536, .F. ) ;
#14742 = CARTESIAN_POINT ( 'NONE',  ( -0.2819296736111110424, 4.967444444520310753, 0.1167790944451424923 ) ) ;
#14743 = CARTESIAN_POINT ( 'NONE',  ( -0.1570231241692966462, 4.178164908778625453, 0.2726904212700292374 ) ) ;
#14744 = DIRECTION ( 'NONE',  ( 0.000000000000000000, 0.000000000000000000, 1.000000000000000000 ) ) ;
#14745 = CARTESIAN_POINT ( 'NONE',  ( 1.397631139260601341, 2.978485840173427324, -2.174029041877829638 ) ) ;
#14746 = CARTESIAN_POINT ( 'NONE',  ( -0.4805263112511646284, 0.2592867110628496174, 0.04342012612512790443 ) ) ;
#14747 = CARTESIAN_POINT ( 'NONE',  ( 0.1292346314604058410, 4.623694444444443441, 0.3119999999999998885 ) ) ;
#14748 = CARTESIAN_POINT ( 'NONE',  ( -0.1993543840281266910, 4.068138888964754507, -0.1993543840281266910 ) ) ;
#14749 = CARTESIAN_POINT ( 'NONE',  ( 0.000000000000000000, 5.384999999999999787, -0.3119999999999999996 ) ) ;
#14750 = CARTESIAN_POINT ( 'NONE',  ( 0.2972964765959422717, 4.032653405754279774, -0.09468309758334170212 ) ) ;
#14751 = CARTESIAN_POINT ( 'NONE',  ( 0.009375000000009008072, 0.5358532185916163870, 0.06112444011295854740 ) ) ;
#14752 = ORIENTED_EDGE ( 'NONE', *, *, #20202, .T. ) ;
#14753 = CARTESIAN_POINT ( 'NONE',  ( 0.003401740878768560843, -0.5383620901250334434, 0.05893285591566548021 ) ) ;
#14754 = ORIENTED_EDGE ( 'NONE', *, *, #2472, .T. ) ;
#14755 = CARTESIAN_POINT ( 'NONE',  ( 0.000000000000000000, 2.735000000000000320, 0.000000000000000000 ) ) ;
#14756 = VECTOR ( 'NONE', #20422, 39.37007874015748854 ) ;
#14757 = CARTESIAN_POINT ( 'NONE',  ( -0.09798969090666245774, -0.2586227216849166788, -0.06558227484231510251 ) ) ;
#14758 = CARTESIAN_POINT ( 'NONE',  ( -3.385114897866767815E-17, -0.2764156081756484196, 0.1577777777777801815 ) ) ;
#14759 = FACE_OUTER_BOUND ( 'NONE', #9435, .T. ) ;
#14760 = CARTESIAN_POINT ( 'NONE',  ( -1.910449006669871087E-17, 4.259111111111110404, -0.3119999999999999996 ) ) ;
#14761 = EDGE_CURVE ( 'NONE', #14781, #3473, #6126, .T. ) ;
#14762 = CARTESIAN_POINT ( 'NONE',  ( -0.4749999999999999778, 3.700000000000000622, -0.09499999999999995948 ) ) ;
#14763 = CARTESIAN_POINT ( 'NONE',  ( 0.3613381517857143232, 0.2258928570453146989, 0.000000000000000000 ) ) ;
#14764 = CARTESIAN_POINT ( 'NONE',  ( -0.1993543840281266633, 0.2784722221463555858, -0.1993543840281266910 ) ) ;
#14765 = CARTESIAN_POINT ( 'NONE',  ( 0.4687500000000002776, -0.1725690304443678602, 0.06591562201456047099 ) ) ;
#14766 = CARTESIAN_POINT ( 'NONE',  ( 0.3003475124358241377, 0.9548081934128058723, 3.454202664143258605 ) ) ;
#14767 = CARTESIAN_POINT ( 'NONE',  ( -0.1585368710484967580, 0.5142162655923535608, -0.7331154209853633086 ) ) ;
#14768 = CARTESIAN_POINT ( 'NONE',  ( -0.1144950937579609918, -0.2764156081756484196, -0.1165277777777775636 ) ) ;
#14769 = ORIENTED_EDGE ( 'NONE', *, *, #16335, .T. ) ;
#14770 = ORIENTED_EDGE ( 'NONE', *, *, #6726, .F. ) ;
#14771 =( BOUNDED_CURVE ( )  B_SPLINE_CURVE ( 2, ( #8478, #15920, #12530, #5182, #19949, #17636, #3239, #8847, #7027 ),
 .UNSPECIFIED., .F., .T. ) 
 B_SPLINE_CURVE_WITH_KNOTS ( ( 3, 2, 2, 2, 3 ),
 ( 0.3125000000000000000, 0.3229166666666666852, 0.3333333333333333148, 0.3437500000000000000, 0.3541666666666666852 ),
 .UNSPECIFIED. ) 
 CURVE ( )  GEOMETRIC_REPRESENTATION_ITEM ( )  RATIONAL_B_SPLINE_CURVE ( ( 1.000000000000000000, 0.9238795325112867385, 1.000000000000000000, 0.9238795325112867385, 1.000000000000000000, 0.9238795325112867385, 1.000000000000000000, 0.9238795325112867385, 1.000000000000000000 ) ) 
 REPRESENTATION_ITEM ( '' )  );
#14772 = CARTESIAN_POINT ( 'NONE',  ( -0.3083781185080407550, 5.106384284016617592, 0.03939064032742058130 ) ) ;
#14773 =( BOUNDED_CURVE ( )  B_SPLINE_CURVE ( 2, ( #262, #13575, #16852, #15149, #4161, #5632, #499 ),
 .UNSPECIFIED., .F., .F. ) 
 B_SPLINE_CURVE_WITH_KNOTS ( ( 3, 2, 2, 3 ),
 ( 0.07506635404883826856, 0.08571428571428571508, 0.1000000000000000056, 0.1071428571428571508 ),
 .UNSPECIFIED. ) 
 CURVE ( )  GEOMETRIC_REPRESENTATION_ITEM ( )  RATIONAL_B_SPLINE_CURVE ( ( 0.9814209735438260696, 0.9635197191029298835, 1.000000000000000000, 0.9510565162951535312, 1.000000000000000000, 0.9755282581475768211, 0.9755282581475768211 ) ) 
 REPRESENTATION_ITEM ( '' )  );
#14774 = CARTESIAN_POINT ( 'NONE',  ( 0.1292346314604057023, 0.007638888888888556439, 0.3119999999999998885 ) ) ;
#14775 = CARTESIAN_POINT ( 'NONE',  ( -0.2819296736111110424, 3.918833333409198705, -0.1167790944451423119 ) ) ;
#14776 = AXIS2_PLACEMENT_3D ( 'NONE', #18013, #14114, #10345 ) ;
#14777 = CARTESIAN_POINT ( 'NONE',  ( 0.2923287055106771337, 0.2187499999024575537, 0.2123892367102621359 ) ) ;
#14778 = CARTESIAN_POINT ( 'NONE',  ( -0.1167790944451423535, 4.377166666742532186, 0.2819296736111110424 ) ) ;
#14779 = CARTESIAN_POINT ( 'NONE',  ( 0.2206173157302027676, 0.1152777776260448528, 0.2206173157302028787 ) ) ;
#14780 = CARTESIAN_POINT ( 'NONE',  ( -0.1166234456863465552, 3.066692553488282957, 2.711183489075826181 ) ) ;
#14781 = VERTEX_POINT ( 'NONE', #13594 ) ;
#14782 = CARTESIAN_POINT ( 'NONE',  ( 0.2824780601149360915, 4.367251178688803748, -0.1354494196218661295 ) ) ;
#14783 = CARTESIAN_POINT ( 'NONE',  ( -0.1993543840281266355, 4.859805555631421470, 0.1993543840281267465 ) ) ;
#14784 = CARTESIAN_POINT ( 'NONE',  ( -0.2605107293023110615, 5.151385429156462692, -0.1530708234642420562 ) ) ;
#14785 = CARTESIAN_POINT ( 'NONE',  ( 0.1236067977499789028, 0.2339285712334865930, 0.3804226065180614791 ) ) ;
#14786 = APPROVAL ( #614, 'UNSPECIFIED' ) ;
#14787 = DIRECTION ( 'NONE',  ( 0.000000000000000000, 0.000000000000000000, -1.000000000000000000 ) ) ;
#14788 = CARTESIAN_POINT ( 'NONE',  ( 0.1993543840281267465, 4.762583333409199149, 0.1993543840281266633 ) ) ;
#14789 = SECURITY_CLASSIFICATION_LEVEL ( 'unclassified' ) ;
#14790 = CARTESIAN_POINT ( 'NONE',  ( -0.1292346314604044810, 4.783416666666666650, 0.3120000000000012208 ) ) ;
#14791 = CARTESIAN_POINT ( 'NONE',  ( 0.000000000000000000, 5.384999999999999787, 0.000000000000000000 ) ) ;
#14792 = CARTESIAN_POINT ( 'NONE',  ( 0.1167790944451423257, 0.5041666665908002276, -0.2819296736111110424 ) ) ;
#14793 = ORIENTED_EDGE ( 'NONE', *, *, #34, .T. ) ;
#14794 = ORIENTED_EDGE ( 'NONE', *, *, #3399, .F. ) ;
#14795 = CARTESIAN_POINT ( 'NONE',  ( -0.2819296736111110979, 0.2437499999241333759, -3.452642723725051716E-17 ) ) ;
#14796 = CARTESIAN_POINT ( 'NONE',  ( -0.2206173157302027676, 4.335499999999998799, 0.2206173157302028787 ) ) ;
#14797 = CARTESIAN_POINT ( 'NONE',  ( -0.2838685103340625182, 5.200889060888042259, -0.02438439758188335263 ) ) ;
#14798 = CARTESIAN_POINT ( 'NONE',  ( -0.2472135954999579444, 0.06785714285714283811, -0.3402603233408159622 ) ) ;
#14799 = CARTESIAN_POINT ( 'NONE',  ( 0.3155070326520292290, 0.1306872919485615736, -0.01756944444444362430 ) ) ;
#14800 = CARTESIAN_POINT ( 'NONE',  ( -0.3104386443325958256, -0.3620340424929879286, 0.08855526556985501840 ) ) ;
#14801 = DIRECTION ( 'NONE',  ( 0.8660254037844384856, 0.000000000000000000, -0.5000000000000003331 ) ) ;
#14802 = CARTESIAN_POINT ( 'NONE',  ( 1.011880822804989588, 2.476536290232590698, -1.198199922892767333 ) ) ;
#14803 = CARTESIAN_POINT ( 'NONE',  ( -0.1993543840281266910, 4.526472222298087544, -0.1993543840281266910 ) ) ;
#14804 = CARTESIAN_POINT ( 'NONE',  ( 0.1236067977499789861, 0.1196428569477723663, -0.3804226065180614236 ) ) ;
#14805 = CARTESIAN_POINT ( 'NONE',  ( 0.1281033428157181131, 4.540104105756370245, -0.2863062090479261412 ) ) ;
#14806 = CARTESIAN_POINT ( 'NONE',  ( 5.178964085587577574E-17, 5.102861111186976828, 0.2819296736111110979 ) ) ;
#14807 = CARTESIAN_POINT ( 'NONE',  ( 0.2819296736111110979, 4.380638888964754507, -3.452642723725051716E-17 ) ) ;
#14808 = CARTESIAN_POINT ( 'NONE',  ( 0.1943347089597592114, 3.744229887717848815, 0.2454019012448671322 ) ) ;
#14809 = CARTESIAN_POINT ( 'NONE',  ( 1.573500000000000343, 2.740000000000000213, -0.9500000000000008438 ) ) ;
#14810 = AXIS2_PLACEMENT_3D ( 'NONE', #6848, #12238, #4537 ) ;
#14811 = CARTESIAN_POINT ( 'NONE',  ( 0.2450140762121532367, 3.912827427306669215, 0.1969830315022409462 ) ) ;
#14812 = CARTESIAN_POINT ( 'NONE',  ( -0.2206173157302028232, 4.050777777929510215, -0.2206173157302028232 ) ) ;
#14813 = CARTESIAN_POINT ( 'NONE',  ( -0.1993543840281266910, 4.526472222298087544, -0.1993543840281266910 ) ) ;
#14814 = CARTESIAN_POINT ( 'NONE',  ( 0.1167790944451424368, 3.925777777853643347, 0.2819296736111110424 ) ) ;
#14815 = EDGE_CURVE ( 'NONE', #13733, #769, #18813, .T. ) ;
#14816 = ORIENTED_EDGE ( 'NONE', *, *, #23915, .F. ) ;
#14817 = PERSON_AND_ORGANIZATION ( #15518, #2538 ) ;
#14818 = CARTESIAN_POINT ( 'NONE',  ( 0.09493784612953225233, -0.2937490000082154662, 0.4199197862486553356 ) ) ;
#14819 = VECTOR ( 'NONE', #10396, 39.37007874015748854 ) ;
#14820 = CARTESIAN_POINT ( 'NONE',  ( -4.760580627680044823E-09, 4.932722222506802368, -0.3119999999999999996 ) ) ;
#14821 = DIRECTION ( 'NONE',  ( 0.000000000000000000, 1.000000000000000000, -1.493785812010397437E-17 ) ) ;
#14822 = ORIENTED_EDGE ( 'NONE', *, *, #21273, .F. ) ;
#14823 = CARTESIAN_POINT ( 'NONE',  ( 1.910449006669871087E-17, 0.5249999998482670627, -0.3119999999999999996 ) ) ;
#14824 = AXIS2_PLACEMENT_3D ( 'NONE', #15271, #3931, #20515 ) ;
#14825 = CARTESIAN_POINT ( 'NONE',  ( 4.422035572083168519E-06, 4.266055436896041719, -0.3120000000040196175 ) ) ;
#14826 = CARTESIAN_POINT ( 'NONE',  ( 0.7919466436700954848, 0.05000000000000028727, -2.986000000000000210 ) ) ;
#14827 = CARTESIAN_POINT ( 'NONE',  ( 0.3613381517857143232, -0.07410714295468522061, -0.1174058825155740587 ) ) ;
#14828 = CARTESIAN_POINT ( 'NONE',  ( 0.08160588755459347032, 3.962804008186619154, 0.3038914485545370359 ) ) ;
#14829 = ORIENTED_EDGE ( 'NONE', *, *, #11755, .F. ) ;
#14830 = VERTEX_POINT ( 'NONE', #7723 ) ;
#14831 = CARTESIAN_POINT ( 'NONE',  ( 0.2233192592356399164, 0.07232142847388617346, 0.3073725909049500604 ) ) ;
#14832 = ORIENTED_EDGE ( 'NONE', *, *, #16291, .T. ) ;
#14833 = CARTESIAN_POINT ( 'NONE',  ( 0.2615970440521218077, 5.090933575972008462, -0.1701841655577382706 ) ) ;
#14834 = CARTESIAN_POINT ( 'NONE',  ( -0.1144950937579609918, -0.2764156081756484196, 0.2654166666666700203 ) ) ;
#14835 = CARTESIAN_POINT ( 'NONE',  ( -0.2819296736111110424, 4.182722222298087544, -0.1167790944451423119 ) ) ;
#14836 = CARTESIAN_POINT ( 'NONE',  ( 0.2819296736111110979, 5.047305555631421470, -3.452642723725051716E-17 ) ) ;
#14837 = EDGE_CURVE ( 'NONE', #16949, #17585, #13474, .T. ) ;
#14838 = CARTESIAN_POINT ( 'NONE',  ( 9.184850993605150903E-17, 3.669999999999999929, -0.7500000000000001110 ) ) ;
#14839 = CARTESIAN_POINT ( 'NONE',  ( -0.3118931856306824124, 4.223187597109412827, -0.04158228275762527321 ) ) ;
#14840 = CARTESIAN_POINT ( 'NONE',  ( -0.3119999999999999996, 3.828555555555555046, 0.000000000000000000 ) ) ;
#14841 = EDGE_CURVE ( 'NONE', #1725, #4460, #7994, .T. ) ;
#14842 = CARTESIAN_POINT ( 'NONE',  ( -0.3119999999999999996, 5.054250000151731648, -0.1292346314604056468 ) ) ;
#14843 = CARTESIAN_POINT ( 'NONE',  ( 0.2065105149757635039, 4.800239184964532058, 0.2355781109500581227 ) ) ;
#14844 = AXIS2_PLACEMENT_3D ( 'NONE', #13303, #2065, #20838 ) ;
#14845 = DIRECTION ( 'NONE',  ( 0.8660254037844361541, 0.000000000000000000, 0.5000000000000042188 ) ) ;
#14846 = EDGE_LOOP ( 'NONE', ( #5779, #19283, #20308, #19901 ) ) ;
#14847 = CARTESIAN_POINT ( 'NONE',  ( 0.3084175934503982641, -2.427762526784286478E-18, -0.1882653658700420007 ) ) ;
#14848 = EDGE_CURVE ( 'NONE', #2585, #16983, #8838, .T. ) ;
#14849 = CARTESIAN_POINT ( 'NONE',  ( 0.2739954178377071448, 0.03290028280361406710, 0.07218012553276310916 ) ) ;
#14850 = ORIENTED_EDGE ( 'NONE', *, *, #17076, .T. ) ;
#14851 = CARTESIAN_POINT ( 'NONE',  ( 0.2230971623002953874, -0.2230971623002954429, 0.3088194444444482545 ) ) ;
#14852 = CARTESIAN_POINT ( 'NONE',  ( 5.178964085587577574E-17, 5.144527777853643791, 0.2819296736111110979 ) ) ;
#14853 = CARTESIAN_POINT ( 'NONE',  ( 0.1580560128843781220, -0.4500121957794399052, 0.4142946745564982103 ) ) ;
#14854 = EDGE_CURVE ( 'NONE', #1954, #5136, #8772, .T. ) ;
#14855 = CYLINDRICAL_SURFACE ( 'NONE', #21925, 0.3125000000000000000 ) ;
#14856 = VECTOR ( 'NONE', #18089, 39.37007874015748143 ) ;
#14857 = CARTESIAN_POINT ( 'NONE',  ( -5.178964085587577574E-17, 0.3687499999241333204, 0.2819296736111110979 ) ) ;
#14858 = CARTESIAN_POINT ( 'NONE',  ( -0.1954553509668046918, -0.1954553509668046640, 0.2133333333333361503 ) ) ;
#14859 = CARTESIAN_POINT ( 'NONE',  ( -0.1167790944451423535, 5.043833333409199149, 0.2819296736111110424 ) ) ;
#14860 = CARTESIAN_POINT ( 'NONE',  ( 0.09811062177514703886, 4.485527722901675673, -0.2964682546474478597 ) ) ;
#14861 = CARTESIAN_POINT ( 'NONE',  ( 0.2819296736111110979, 4.988277777853642903, 0.1167790944451422425 ) ) ;
#14862 = CARTESIAN_POINT ( 'NONE',  ( 0.3860879860166684940, 4.111524471938507119, -2.831872695974971599 ) ) ;
#14863 = EDGE_CURVE ( 'NONE', #20713, #17619, #8651, .T. ) ;
#14864 = DIRECTION ( 'NONE',  ( 0.5000000000000005551, -0.000000000000000000, 0.8660254037844383745 ) ) ;
#14865 = CARTESIAN_POINT ( 'NONE',  ( 2.160501146175418441, 2.291712385858714729, -2.201288568297000925 ) ) ;
#14866 = CARTESIAN_POINT ( 'NONE',  ( 1.889965290469428183, 2.453197021783230181, -1.916312967630974695 ) ) ;
#14867 = CARTESIAN_POINT ( 'NONE',  ( -0.2206173157302027676, 4.446611111111110404, 0.2206173157302028787 ) ) ;
#14868 = ADVANCED_FACE ( 'NONE', ( #14271 ), #23135, .F. ) ;
#14869 = CARTESIAN_POINT ( 'NONE',  ( -0.1993543840281266910, 3.957027777853642903, -0.1993543840281266910 ) ) ;
#14870 = FACE_BOUND ( 'NONE', #15133, .T. ) ;
#14871 = CARTESIAN_POINT ( 'NONE',  ( 0.3092439325280461060, 4.031202289993226273, -0.04474935879389044247 ) ) ;
#14872 = CARTESIAN_POINT ( 'NONE',  ( -0.1056007431694158949, 3.735235609415689773, 0.2935856185260024565 ) ) ;
#14873 = CARTESIAN_POINT ( 'NONE',  ( -0.1292346314604081725, 4.561194444444443441, 0.3119999999999974460 ) ) ;
#14874 = VERTEX_POINT ( 'NONE', #235 ) ;
#14875 = CARTESIAN_POINT ( 'NONE',  ( -0.1746005203414776330, 4.121880983008269439, 0.2585734667409969600 ) ) ;
#14876 = CARTESIAN_POINT ( 'NONE',  ( 0.03061863295597656159, 4.154064737224905102, -0.3119999618532416918 ) ) ;
#14877 = CARTESIAN_POINT ( 'NONE',  ( 0.000000000000000000, 0.2764156081756484196, 0.2411111111111142458 ) ) ;
#14878 = LINE ( 'NONE', #18519, #14611 ) ;
#14879 = DIRECTION ( 'NONE',  ( -0.000000000000000000, -1.000000000000000000, -0.000000000000000000 ) ) ;
#14880 = CARTESIAN_POINT ( 'NONE',  ( 0.2923287055106771337, 0.2901785713310289783, 0.2123892367102621359 ) ) ;
#14881 = CARTESIAN_POINT ( 'NONE',  ( 1.726321361862525858E-17, 0.1604166665908000333, -0.2819296736111110979 ) ) ;
#14882 = LINE ( 'NONE', #10739, #17786 ) ;
#14883 = CARTESIAN_POINT ( 'NONE',  ( -0.3125000000000000000, 1.913510623667739771E-17, 0.06055555555555702796 ) ) ;
#14884 = CARTESIAN_POINT ( 'NONE',  ( 0.2764156081756483641, 0.1144950937579610056, -0.09569444444444405451 ) ) ;
#14885 = VERTEX_POINT ( 'NONE', #3893 ) ;
#14886 = DIRECTION ( 'NONE',  ( 0.4999999999999908962, 0.000000000000000000, -0.8660254037844438146 ) ) ;
#14887 = CARTESIAN_POINT ( 'NONE',  ( 0.000000000000000000, 5.384999999999999787, 0.000000000000000000 ) ) ;
#14888 = CARTESIAN_POINT ( 'NONE',  ( -0.2206173157302027954, 0.03888888888888855644, -0.2206173157302028232 ) ) ;
#14889 = CARTESIAN_POINT ( 'NONE',  ( 0.1292346314604056190, 5.255638888888888083, -0.3119999999999999996 ) ) ;
#14890 = CARTESIAN_POINT ( 'NONE',  ( -0.1116596296178200276, 0.2758928570453147433, 0.3436530038418508792 ) ) ;
#14891 = VERTEX_POINT ( 'NONE', #20358 ) ;
#14892 = CARTESIAN_POINT ( 'NONE',  ( 0.2819296736111110979, 4.505638888964754507, -3.452642723725051716E-17 ) ) ;
#14893 = CARTESIAN_POINT ( 'NONE',  ( 0.000000000000000000, 0.4202679491924311006, 0.000000000000000000 ) ) ;
#14894 = DIRECTION ( 'NONE',  ( -0.000000000000000000, -1.000000000000000000, -0.000000000000000000 ) ) ;
#14895 = EDGE_CURVE ( 'NONE', #5067, #19113, #18725, .T. ) ;
#14896 = CARTESIAN_POINT ( 'NONE',  ( -0.2819296736111110424, 5.023000000075864335, 0.1167790944451424923 ) ) ;
#14897 = CARTESIAN_POINT ( 'NONE',  ( -0.2851947699491957922, 5.157899255522624848, 0.09432962184258192329 ) ) ;
#14898 = DIRECTION ( 'NONE',  ( 0.000000000000000000, 1.000000000000000000, 0.000000000000000000 ) ) ;
#14899 = CARTESIAN_POINT ( 'NONE',  ( 0.000000000000000000, 0.4987679491924311148, 0.2510000000000000009 ) ) ;
#14900 = CARTESIAN_POINT ( 'NONE',  ( 0.2819296736111111534, 4.766055555631421470, 0.1167790944451422563 ) ) ;
#14901 = SECURITY_CLASSIFICATION_LEVEL ( 'unclassified' ) ;
#14902 = CARTESIAN_POINT ( 'NONE',  ( -0.4788584550258518369, 0.2689697488930834490, 0.04193801346286365334 ) ) ;
#14903 = CARTESIAN_POINT ( 'NONE',  ( -0.3120000000000000551, 0.4312499998482670072, 0.1292346314604056190 ) ) ;
#14904 =( BOUNDED_CURVE ( )  B_SPLINE_CURVE ( 2, ( #3840, #5900, #13008, #14941, #15065, #20304, #24067, #9326, #16766 ),
 .UNSPECIFIED., .F., .F. ) 
 B_SPLINE_CURVE_WITH_KNOTS ( ( 3, 2, 2, 2, 3 ),
 ( 0.7708333333333333703, 0.7812500000000000000, 0.7916666666666666297, 0.8020833333333333703, 0.8125000000000000000 ),
 .UNSPECIFIED. ) 
 CURVE ( )  GEOMETRIC_REPRESENTATION_ITEM ( )  RATIONAL_B_SPLINE_CURVE ( ( 1.000000000000000000, 0.9238795325112867385, 1.000000000000000000, 0.9238795325112867385, 1.000000000000000000, 0.9238795325112867385, 1.000000000000000000, 0.9238795325112867385, 1.000000000000000000 ) ) 
 REPRESENTATION_ITEM ( '' )  );
#14905 = CARTESIAN_POINT ( 'NONE',  ( 0.1167790944451423535, 0.4833333332574667462, 0.2819296736111110424 ) ) ;
#14906 = VERTEX_POINT ( 'NONE', #3775 ) ;
#14907 = ORIENTED_EDGE ( 'NONE', *, *, #21071, .T. ) ;
#14908 = CARTESIAN_POINT ( 'NONE',  ( 0.1993543840281266910, 0.1673611110352444808, -0.1993543840281266910 ) ) ;
#14909 = DIRECTION ( 'NONE',  ( 1.000000000000000000, 0.000000000000000000, -1.224646799147353207E-16 ) ) ;
#14910 = CARTESIAN_POINT ( 'NONE',  ( 0.2510000000000000009, 5.500232050807569273, 0.000000000000000000 ) ) ;
#14911 = CARTESIAN_POINT ( 'NONE',  ( 0.1236067977499789861, 0.1285714285714285310, -0.3804226065180614236 ) ) ;
#14912 = CARTESIAN_POINT ( 'NONE',  ( -0.3155070326520292845, 1.931923388228935888E-17, 0.006736111111112118993 ) ) ;
#14913 = VECTOR ( 'NONE', #2173, 39.37007874015748854 ) ;
#14914 = DIRECTION ( 'NONE',  ( 0.000000000000000000, 0.000000000000000000, -1.000000000000000000 ) ) ;
#14915 = DIRECTION ( 'NONE',  ( 0.000000000000000000, -1.000000000000000000, 0.000000000000000000 ) ) ;
#14916 = CARTESIAN_POINT ( 'NONE',  ( -0.2819296736111111534, 0.3444444443685778512, 0.1167790944451422563 ) ) ;
#14917 = CARTESIAN_POINT ( 'NONE',  ( 1.047989435620467535, 2.471736157945124912, -1.135238013746948438 ) ) ;
#14918 = CARTESIAN_POINT ( 'NONE',  ( 0.1167790944451424368, 4.606333333409200037, 0.2819296736111110424 ) ) ;
#14919 = CARTESIAN_POINT ( 'NONE',  ( -0.1236067977499789583, -0.01607142876651335150, -0.3804226065180614791 ) ) ;
#14920 = CARTESIAN_POINT ( 'NONE',  ( 0.2434586614536247695, 1.857579423845308038E-17, -0.2752667295144964332 ) ) ;
#14921 = CARTESIAN_POINT ( 'NONE',  ( 0.1993543840281267465, 5.165361111186976828, 0.1993543840281266633 ) ) ;
#14922 = CC_DESIGN_PERSON_AND_ORGANIZATION_ASSIGNMENT ( #16331, #5685, ( #9710 ) ) ;
#14923 = CARTESIAN_POINT ( 'NONE',  ( -0.2819296736111110979, 4.519527777853643791, 0.000000000000000000 ) ) ;
#14924 = CARTESIAN_POINT ( 'NONE',  ( 0.03254485797104954281, 3.739221291613469500, 0.3108638213126159733 ) ) ;
#14925 = CARTESIAN_POINT ( 'NONE',  ( -0.4224880990050804974, 0.2973422596752779423, 0.07046568677125501778 ) ) ;
#14926 = CARTESIAN_POINT ( 'NONE',  ( 0.3119999999999999996, 4.088972222373953969, -0.1292346314604056745 ) ) ;
#14927 = CARTESIAN_POINT ( 'NONE',  ( -0.1993543840281266910, 4.582027777853643791, -0.1993543840281266910 ) ) ;
#14928 = DIRECTION ( 'NONE',  ( 0.4999999999999918954, 0.000000000000000000, 0.8660254037844432595 ) ) ;
#14929 = AXIS2_PLACEMENT_3D ( 'NONE', #6143, #9575, #6022 ) ;
#14930 = CARTESIAN_POINT ( 'NONE',  ( 0.2879402880768414108, -0.08326397218404227307, -0.08843619990776636908 ) ) ;
#14931 = EDGE_LOOP ( 'NONE', ( #22796, #1844, #4293, #12266 ) ) ;
#14932 = VERTEX_POINT ( 'NONE', #20241 ) ;
#14933 = APPROVAL_ROLE ( '' ) ;
#14934 = CARTESIAN_POINT ( 'NONE',  ( -0.1246856373887775538, 4.845749071750494963, 0.2860203695084122533 ) ) ;
#14935 = FACE_OUTER_BOUND ( 'NONE', #21672, .T. ) ;
#14936 = ORIENTED_EDGE ( 'NONE', *, *, #6901, .T. ) ;
#14937 = CARTESIAN_POINT ( 'NONE',  ( 0.2206173157302027676, 0.5597222220704892726, 0.2206173157302028787 ) ) ;
#14938 = CARTESIAN_POINT ( 'NONE',  ( 0.1294417382415921358, -0.3125000000000002220, 0.1959722222222251287 ) ) ;
#14939 = CARTESIAN_POINT ( 'NONE',  ( 0.000000000000000000, 0.8949999999999999067, 0.000000000000000000 ) ) ;
#14940 = CARTESIAN_POINT ( 'NONE',  ( -0.2923287055106771337, -0.04910714295468524004, -0.2123892367102620804 ) ) ;
#14941 = CARTESIAN_POINT ( 'NONE',  ( -0.3119999999999999996, 0.4868055555555551583, -0.1292346314604056745 ) ) ;
#14942 = EDGE_LOOP ( 'NONE', ( #4997, #7845, #15161, #11249 ) ) ;
#14943 = CARTESIAN_POINT ( 'NONE',  ( 0.2923287055106771337, 0.09017857133102902267, -0.2123892367102620249 ) ) ;
#14944 = VERTEX_POINT ( 'NONE', #7549 ) ;
#14945 = DIRECTION ( 'NONE',  ( -1.000000000000000000, 0.000000000000000000, 0.000000000000000000 ) ) ;
#14946 = CARTESIAN_POINT ( 'NONE',  ( -0.1144950937579609779, 0.2764156081756484196, 0.2445833333333364834 ) ) ;
#14947 = APPROVAL ( #1521, 'UNSPECIFIED' ) ;
#14948 = VECTOR ( 'NONE', #2324, 39.37007874015748143 ) ;
#14949 = ADVANCED_FACE ( 'NONE', ( #11338 ), #11095, .T. ) ;
#14950 = CARTESIAN_POINT ( 'NONE',  ( -0.1167790944451423535, 4.252166666742533074, 0.2819296736111110424 ) ) ;
#14951 = CARTESIAN_POINT ( 'NONE',  ( 0.2819296736111110979, 5.102861111186976828, -3.452642723725051716E-17 ) ) ;
#14952 = CARTESIAN_POINT ( 'NONE',  ( 0.3050515993604266951, -0.01759458571372691030, 0.4170999431000476099 ) ) ;
#14953 = CARTESIAN_POINT ( 'NONE',  ( 0.000000000000000000, 2.740000000000000213, 0.000000000000000000 ) ) ;
#14954 = CARTESIAN_POINT ( 'NONE',  ( -0.3119999999999999996, 3.936194444444443441, -0.1292346314604056468 ) ) ;
#14955 = CARTESIAN_POINT ( 'NONE',  ( -0.3119999999999999996, 4.832027777929510215, -0.1292346314604056468 ) ) ;
#14956 = CARTESIAN_POINT ( 'NONE',  ( 0.3010077053382372303, 4.805368180615793960, 0.08343459883119609677 ) ) ;
#14957 = DIRECTION ( 'NONE',  ( -0.8660254037844382635, 0.000000000000000000, -0.5000000000000004441 ) ) ;
#14958 = EDGE_LOOP ( 'NONE', ( #15608, #15343, #16599, #5532 ) ) ;
#14959 = CARTESIAN_POINT ( 'NONE',  ( 0.2233192592356400275, 0.07589285704531473220, -0.3073725909049499494 ) ) ;
#14960 = CARTESIAN_POINT ( 'NONE',  ( 0.2267002397118211554, 0.03806586609000491700, -0.1772890151010469983 ) ) ;
#14961 = ORIENTED_EDGE ( 'NONE', *, *, #20498, .T. ) ;
#14962 = COORDINATED_UNIVERSAL_TIME_OFFSET ( 0, 0, .AHEAD. ) ;
#14963 = VECTOR ( 'NONE', #13066, 39.37007874015748143 ) ;
#14964 = VERTEX_POINT ( 'NONE', #10981 ) ;
#14965 = CARTESIAN_POINT ( 'NONE',  ( 0.1167790944451422702, 5.057722222298087544, -0.2819296736111110424 ) ) ;
#14966 = CARTESIAN_POINT ( 'NONE',  ( 5.178964085587577574E-17, 3.769527777853644235, 0.2819296736111110979 ) ) ;
#14967 = DIRECTION ( 'NONE',  ( -0.000000000000000000, -1.000000000000000000, -0.000000000000000000 ) ) ;
#14968 = FACE_OUTER_BOUND ( 'NONE', #9717, .T. ) ;
#14969 = VERTEX_POINT ( 'NONE', #18288 ) ;
#14970 = CARTESIAN_POINT ( 'NONE',  ( 0.2764156081756483641, 0.1144950937579610195, 0.008472222222223454655 ) ) ;
#14971 = CARTESIAN_POINT ( 'NONE',  ( -0.1167790944451424506, 0.2541666665908000056, 0.2819296736111110424 ) ) ;
#14972 = CARTESIAN_POINT ( 'NONE',  ( 0.2764156081756483641, -0.1144950937579611167, 0.2862500000000034461 ) ) ;
#14973 = CARTESIAN_POINT ( 'NONE',  ( -0.1993543840281266355, 4.929250000075866112, 0.1993543840281267465 ) ) ;
#14974 = CARTESIAN_POINT ( 'NONE',  ( -0.3236067977499789694, 0.4196428569477722581, -0.2351141009169893104 ) ) ;
#14975 = EDGE_CURVE ( 'NONE', #13117, #10268, #2368, .T. ) ;
#14976 = CARTESIAN_POINT ( 'NONE',  ( 0.1167790944451424368, 4.981333333409198261, 0.2819296736111110424 ) ) ;
#14977 = CARTESIAN_POINT ( 'NONE',  ( -0.4592333586340865414, 0.08963635625773219706, 0.4305718605174581048 ) ) ;
#14978 = LINE ( 'NONE', #13040, #19479 ) ;
#14979 = FACE_OUTER_BOUND ( 'NONE', #15917, .T. ) ;
#14980 = CARTESIAN_POINT ( 'NONE',  ( 0.2386280844052624528, -0.1440056533833775076, 0.3886972078529389862 ) ) ;
#14981 = CARTESIAN_POINT ( 'NONE',  ( -0.1292346314604057023, 4.505638888888887195, 0.3119999999999998885 ) ) ;
#14982 = CARTESIAN_POINT ( 'NONE',  ( -0.4000000000000000222, 0.2928571428571427604, -4.898587196589413075E-17 ) ) ;
#14983 = VECTOR ( 'NONE', #22473, 39.37007874015748854 ) ;
#14984 = CARTESIAN_POINT ( 'NONE',  ( 0.1292346314604057300, 0.3340277776260447418, 0.3119999999999998885 ) ) ;
#14985 = CYLINDRICAL_SURFACE ( 'NONE', #14451, 0.3119999999999999996 ) ;
#14986 = CARTESIAN_POINT ( 'NONE',  ( 0.07901360339605351113, 4.597109866223552110, -0.3045289936772480055 ) ) ;
#14987 = ORIENTED_EDGE ( 'NONE', *, *, #2968, .T. ) ;
#14988 =( GEOMETRIC_REPRESENTATION_CONTEXT ( 3 ) GLOBAL_UNCERTAINTY_ASSIGNED_CONTEXT ( ( #704 ) ) GLOBAL_UNIT_ASSIGNED_CONTEXT ( ( #17589, #8558, #13708 ) ) REPRESENTATION_CONTEXT ( 'NONE', 'WORKASPACE' ) );
#14989 = CARTESIAN_POINT ( 'NONE',  ( -0.1607995357127989244, 4.122348446938056021, 0.2674091126109629513 ) ) ;
#14990 = CARTESIAN_POINT ( 'NONE',  ( 6.388359114324787822E-07, 4.627192232271967853, 0.3119999999985919592 ) ) ;
#14991 = EDGE_CURVE ( 'NONE', #13298, #22303, #3859, .T. ) ;
#14992 = EDGE_CURVE ( 'NONE', #2791, #21366, #1004, .T. ) ;
#14993 = CARTESIAN_POINT ( 'NONE',  ( -0.1954553509668046640, 0.1954553509668046918, 0.1925000000000027245 ) ) ;
#14994 = EDGE_CURVE ( 'NONE', #14330, #6883, #13413, .T. ) ;
#14995 = AXIS2_PLACEMENT_3D ( 'NONE', #21100, #9524, #13567 ) ;
#14996 = CARTESIAN_POINT ( 'NONE',  ( -1.522235971340160240E-16, 0.1799999999999999933, -1.243000000000000105 ) ) ;
#14997 = CARTESIAN_POINT ( 'NONE',  ( 0.2993330080277241678, 5.144326520802546376, 0.05249542264811372927 ) ) ;
#14998 = ORIENTED_EDGE ( 'NONE', *, *, #14007, .T. ) ;
#14999 = CARTESIAN_POINT ( 'NONE',  ( 2.326421213736078119E-17, 0.3866071427596002308, -0.3799334167787516425 ) ) ;
#15000 = CARTESIAN_POINT ( 'NONE',  ( -0.1167790944451422702, 0.1638888888130222432, -0.2819296736111110424 ) ) ;
#15001 = CARTESIAN_POINT ( 'NONE',  ( 0.000000000000000000, 0.3125000000000000000, 0.1647222222222248789 ) ) ;
#15002 = DIRECTION ( 'NONE',  ( 0.08715574274765830465, -0.9961946980917454342, -3.870492493070289564E-17 ) ) ;
#15003 = LINE ( 'NONE', #4014, #18326 ) ;
#15004 = CARTESIAN_POINT ( 'NONE',  ( 0.1954553509668047195, 0.1954553509668046085, -0.03666666666666580643 ) ) ;
#15005 = ADVANCED_FACE ( 'NONE', ( #9871 ), #19242, .T. ) ;
#15006 = ORIENTED_EDGE ( 'NONE', *, *, #19439, .F. ) ;
#15007 = DIRECTION ( 'NONE',  ( 0.000000000000000000, -1.000000000000000000, 0.000000000000000000 ) ) ;
#15008 = CARTESIAN_POINT ( 'NONE',  ( 0.2206173157302028787, 4.349388888888888083, 0.2206173157302027954 ) ) ;
#15009 = CC_DESIGN_APPROVAL ( #19972, ( #9710 ) ) ;
#15010 = CARTESIAN_POINT ( 'NONE',  ( -0.3119999999999999996, 0.1048611111111107663, 0.1292346314604056190 ) ) ;
#15011 = CARTESIAN_POINT ( 'NONE',  ( 0.2206173157302028787, 5.127166666666665762, 0.2206173157302027954 ) ) ;
#15012 = CARTESIAN_POINT ( 'NONE',  ( -0.3613381517857144343, 0.2651785713310289005, 0.1174058825155740171 ) ) ;
#15013 = CARTESIAN_POINT ( 'NONE',  ( -0.1167790944451423535, 4.266055555631421470, 0.2819296736111110424 ) ) ;
#15014 = CARTESIAN_POINT ( 'NONE',  ( 0.2730879860166738338, 4.111524471938507119, -3.027594437230249902 ) ) ;
#15015 = CARTESIAN_POINT ( 'NONE',  ( 0.000000000000000000, 0.000000000000000000, -0.1019043464467004889 ) ) ;
#15016 = ORIENTED_EDGE ( 'NONE', *, *, #15293, .T. ) ;
#15017 = CARTESIAN_POINT ( 'NONE',  ( 0.2472135954999579166, 0.3089285712334864931, 0.3402603233408160732 ) ) ;
#15018 = CARTESIAN_POINT ( 'NONE',  ( -1.726321361862525858E-17, 5.005638888964754507, -0.2819296736111110979 ) ) ;
#15019 = CARTESIAN_POINT ( 'NONE',  ( -2.307748244742446386E-07, 4.182713274783838919, 0.3119999999998222528 ) ) ;
#15020 = CARTESIAN_POINT ( 'NONE',  ( 0.1988756632394131918, 3.704359868413474199, -0.2404006459456452249 ) ) ;
#15021 = CARTESIAN_POINT ( 'NONE',  ( 1.962795215930568826, 2.690142902515285428, -2.659227944919802855 ) ) ;
#15022 = CARTESIAN_POINT ( 'NONE',  ( -0.1167790944451423535, 4.696611111186976828, 0.2819296736111110979 ) ) ;
#15023 = APPROVAL_STATUS ( 'not_yet_approved' ) ;
#15024 = CARTESIAN_POINT ( 'NONE',  ( -0.3119999999999999996, 4.769527777777777366, -0.1292346314604056468 ) ) ;
#15025 = FACE_OUTER_BOUND ( 'NONE', #18114, .T. ) ;
#15026 = CARTESIAN_POINT ( 'NONE',  ( -0.1993543840281267465, 0.4173611110352444253, 0.1993543840281266633 ) ) ;
#15027 = ORIENTED_EDGE ( 'NONE', *, *, #7686, .T. ) ;
#15028 = ORIENTED_EDGE ( 'NONE', *, *, #23584, .F. ) ;
#15029 = CARTESIAN_POINT ( 'NONE',  ( 0.1167790944451423535, 0.3166666665907999501, 0.2819296736111110424 ) ) ;
#15030 = DIRECTION ( 'NONE',  ( -0.000000000000000000, 0.000000000000000000, 1.000000000000000000 ) ) ;
#15031 = CARTESIAN_POINT ( 'NONE',  ( 1.750236327630675475E-17, 0.3374999998049151295, -0.3999999999999999667 ) ) ;
#15032 = VECTOR ( 'NONE', #7641, 39.37007874015748854 ) ;
#15033 = CARTESIAN_POINT ( 'NONE',  ( 0.3236067977499790249, 0.2642857142857141795, -0.2351141009169892826 ) ) ;
#15034 = DIRECTION ( 'NONE',  ( 0.000000000000000000, 0.000000000000000000, -1.000000000000000000 ) ) ;
#15035 = ADVANCED_FACE ( 'NONE', ( #13660 ), #4365, .T. ) ;
#15036 = CARTESIAN_POINT ( 'NONE',  ( 0.4687500000000003886, 0.2173969584302052338, 0.3901935604185519102 ) ) ;
#15037 = CARTESIAN_POINT ( 'NONE',  ( 0.000000000000000000, 5.384999999999999787, -0.3119999999999999996 ) ) ;
#15038 = CARTESIAN_POINT ( 'NONE',  ( 0.1993543840281266910, 0.1534722221463555858, -0.1993543840281266910 ) ) ;
#15039 = CARTESIAN_POINT ( 'NONE',  ( -0.1167790944451424368, 0.07361111103524446697, 0.2819296736111110424 ) ) ;
#15040 = CARTESIAN_POINT ( 'NONE',  ( 0.1993543840281266633, 4.234805555631421470, -0.1993543840281266910 ) ) ;
#15041 = ORIENTED_EDGE ( 'NONE', *, *, #8159, .T. ) ;
#15042 = CARTESIAN_POINT ( 'NONE',  ( -0.2472135954999579444, -0.01250000019508477368, -0.3402603233408159622 ) ) ;
#15043 = CARTESIAN_POINT ( 'NONE',  ( 0.2819296736111110979, 4.835500000075866112, 0.1167790944451422425 ) ) ;
#15044 = CARTESIAN_POINT ( 'NONE',  ( 0.1167790944451424506, 4.425777777853642903, 0.2819296736111110424 ) ) ;
#15045 = CARTESIAN_POINT ( 'NONE',  ( 0.3060819870397865072, 0.9548081934128058723, 2.694270262774470126 ) ) ;
#15046 = CC_DESIGN_APPROVAL ( #3454, ( #11937 ) ) ;
#15047 = EDGE_LOOP ( 'NONE', ( #313, #10664, #11574, #2389 ) ) ;
#15048 = CARTESIAN_POINT ( 'NONE',  ( 0.03189102445560762500, 3.905830426954165269, 0.3119999985971984025 ) ) ;
#15049 = CARTESIAN_POINT ( 'NONE',  ( -0.3119999999999999996, 3.998694444596176734, -0.1292346314604056468 ) ) ;
#15050 = CARTESIAN_POINT ( 'NONE',  ( 0.1797083160605401908, 3.721720973846279534, -0.2172308955953379805 ) ) ;
#15051 = CLOSED_SHELL ( 'NONE', ( #20692, #5290, #6945, #8988, #9787, #8122, #19584, #12911, #21240, #871, #1122, #22991, #2420, #3208, #6191, #16817, #12913, #19006, #14059, #10669, #14697, #10848, #23649, #13783, #17769, #23446, #14710, #7800, #18020, #7221 ) ) ;
#15052 = CARTESIAN_POINT ( 'NONE',  ( -0.2658399375755275962, -0.1645562284205263071, -0.1013565772524682301 ) ) ;
#15053 = ORIENTED_EDGE ( 'NONE', *, *, #11151, .F. ) ;
#15054 = DATE_AND_TIME ( #19177, #19314 ) ;
#15055 = CARTESIAN_POINT ( 'NONE',  ( -0.1764095973158986419, -0.2469329051808260012, 0.4146780700801321329 ) ) ;
#15056 = CARTESIAN_POINT ( 'NONE',  ( 0.2481776206062809020, -0.3871563449089071018, 0.4344098397133765443 ) ) ;
#15057 = PLANE ( 'NONE',  #9677 ) ;
#15058 = APPROVAL_PERSON_ORGANIZATION ( #8403, #10761, #17804 ) ;
#15059 = ORIENTED_EDGE ( 'NONE', *, *, #7665, .T. ) ;
#15060 = CARTESIAN_POINT ( 'NONE',  ( 1.910449006669871087E-17, 0.5805555554038225319, -0.3119999999999999996 ) ) ;
#15061 = ORIENTED_EDGE ( 'NONE', *, *, #21670, .F. ) ;
#15062 = DIRECTION ( 'NONE',  ( -0.8660254037844438146, -0.000000000000000000, -0.4999999999999910627 ) ) ;
#15063 = CARTESIAN_POINT ( 'NONE',  ( 0.03384475192914793845, 4.739198603489362505, 0.3119999968134716806 ) ) ;
#15064 = CARTESIAN_POINT ( 'NONE',  ( -0.2233192592356399442, 0.1616071427596004473, -0.3073725909049500049 ) ) ;
#15065 = CARTESIAN_POINT ( 'NONE',  ( -0.3119999999999999996, 0.4902777777777773682, -3.820898013339742174E-17 ) ) ;
#15066 = VERTEX_POINT ( 'NONE', #832 ) ;
#15067 = CARTESIAN_POINT ( 'NONE',  ( -6.979263641208234666E-17, 0.1366071427596004251, 0.3799334167787516980 ) ) ;
#15068 = ORIENTED_EDGE ( 'NONE', *, *, #22587, .F. ) ;
#15069 = LINE ( 'NONE', #22491, #15367 ) ;
#15070 = CARTESIAN_POINT ( 'NONE',  ( -0.2934967222474210158, 4.665782234535950757, -0.1058913119755514193 ) ) ;
#15071 = CARTESIAN_POINT ( 'NONE',  ( -0.1167790944451423535, 4.141055555631421470, 0.2819296736111110424 ) ) ;
#15072 = LINE ( 'NONE', #7857, #23083 ) ;
#15073 = CARTESIAN_POINT ( 'NONE',  ( -0.4620259694561524855, -0.2880908832651560281, 0.04413116910601651982 ) ) ;
#15074 = CARTESIAN_POINT ( 'NONE',  ( -0.3119999999999998885, 3.832027777777777366, 0.1292346314604058410 ) ) ;
#15075 = CARTESIAN_POINT ( 'NONE',  ( -0.1292346314604057023, 4.734805555707287894, 0.3119999999999998885 ) ) ;
#15076 = CARTESIAN_POINT ( 'NONE',  ( 0.03717498437443090414, 4.794923932970774239, 0.3120000032159864767 ) ) ;
#15077 =( BOUNDED_CURVE ( )  B_SPLINE_CURVE ( 2, ( #5848, #17195, #18904 ),
 .UNSPECIFIED., .F., .F. ) 
 B_SPLINE_CURVE_WITH_KNOTS ( ( 3, 3 ),
 ( 1.734723475976807094E-18, 0.002646478566469968440 ),
 .UNSPECIFIED. ) 
 CURVE ( )  GEOMETRIC_REPRESENTATION_ITEM ( )  RATIONAL_B_SPLINE_CURVE ( ( 1.000000000000000000, 0.4999999999999997780, 1.000000000000000000 ) ) 
 REPRESENTATION_ITEM ( '' )  );
#15078 = CARTESIAN_POINT ( 'NONE',  ( -0.1993543840281266910, 4.179250000075865223, -0.1993543840281266910 ) ) ;
#15079 = PLANE ( 'NONE',  #22962 ) ;
#15080 = EDGE_LOOP ( 'NONE', ( #18732, #6001, #16046, #4766 ) ) ;
#15081 = CARTESIAN_POINT ( 'NONE',  ( 0.3613381517857143232, 0.1330357141881718941, 0.1174058825155741975 ) ) ;
#15082 = ORIENTED_EDGE ( 'NONE', *, *, #16857, .T. ) ;
#15083 = CONICAL_SURFACE ( 'NONE', #2217, 0.3119999999999999996, 0.7853981633974450594 ) ;
#15084 = APPROVAL_DATE_TIME ( #21695, #8045 ) ;
#15085 = CC_DESIGN_PERSON_AND_ORGANIZATION_ASSIGNMENT ( #7453, #2456, ( #11949 ) ) ;
#15086 = CARTESIAN_POINT ( 'NONE',  ( 0.3155070326520292290, 0.1306872919485615736, 0.3747916666666710750 ) ) ;
#15087 = CARTESIAN_POINT ( 'NONE',  ( -1.726321361862525858E-17, 5.061194444520309865, -0.2819296736111110979 ) ) ;
#15088 = CARTESIAN_POINT ( 'NONE',  ( -1.726321361862525858E-17, 3.908416666742532630, -0.2819296736111110979 ) ) ;
#15089 = CARTESIAN_POINT ( 'NONE',  ( 0.07516378717669286447, 4.407066051533294448, 0.3028153355424372806 ) ) ;
#15090 = CARTESIAN_POINT ( 'NONE',  ( 0.1961225106001930063, -0.4280344930761078581, 0.09139053646024343502 ) ) ;
#15091 = EDGE_LOOP ( 'NONE', ( #3085, #23128, #5486, #9861, #9966, #5411, #22314 ) ) ;
#15092 = CARTESIAN_POINT ( 'NONE',  ( 0.1144950937579609085, -0.2764156081756484751, 0.2723611111111144956 ) ) ;
#15093 = CARTESIAN_POINT ( 'NONE',  ( 0.2819296736111110979, 0.4937499999241333759, 0.000000000000000000 ) ) ;
#15094 = CARTESIAN_POINT ( 'NONE',  ( -0.2764156081756484196, -0.1144950937579609362, -0.07486111111111054539 ) ) ;
#15095 = CARTESIAN_POINT ( 'NONE',  ( -0.2819296736111110979, 4.866750000075866112, 0.000000000000000000 ) ) ;
#15096 = CYLINDRICAL_SURFACE ( 'NONE', #3078, 0.3125000000000000000 ) ;
#15097 = CARTESIAN_POINT ( 'NONE',  ( 0.1993543840281266633, 4.943138888964754507, -0.1993543840281266910 ) ) ;
#15098 = CARTESIAN_POINT ( 'NONE',  ( 0.000000000000000000, 0.04579999999999925103, 0.000000000000000000 ) ) ;
#15099 = CARTESIAN_POINT ( 'NONE',  ( -0.5116234456863466562, 3.514980167629567998, 2.722575290337332365 ) ) ;
#15100 = DIRECTION ( 'NONE',  ( -0.000000000000000000, -1.000000000000000000, -0.000000000000000000 ) ) ;
#15101 = LINE ( 'NONE', #2293, #18974 ) ;
#15102 = CARTESIAN_POINT ( 'NONE',  ( 0.3119999999999999996, 4.519527777777776478, 0.1292346314604056190 ) ) ;
#15103 = AXIS2_PLACEMENT_3D ( 'NONE', #22282, #14616, #10839 ) ;
#15104 = CARTESIAN_POINT ( 'NONE',  ( -0.3236067977499790249, 0.2999999999999999334, 0.2351141009169892271 ) ) ;
#15105 = CARTESIAN_POINT ( 'NONE',  ( 5.731347020009612645E-17, 4.231333333333332725, 0.3119999999999999996 ) ) ;
#15106 = CARTESIAN_POINT ( 'NONE',  ( 0.04766631159125447187, 4.986907329414384193, -0.3085658132919876229 ) ) ;
#15107 = CARTESIAN_POINT ( 'NONE',  ( -0.1053467703269967554, 3.735243447484689394, 0.2936768054724072097 ) ) ;
#15108 = CARTESIAN_POINT ( 'NONE',  ( -0.4593750000000004219, 0.2760455974562897596, 0.4425000000000000044 ) ) ;
#15109 = ORIENTED_EDGE ( 'NONE', *, *, #17465, .T. ) ;
#15110 = CARTESIAN_POINT ( 'NONE',  ( -0.02675153519987890152, 4.126403458700751870, 0.3120000000339450130 ) ) ;
#15111 = EDGE_CURVE ( 'NONE', #19709, #404, #19125, .T. ) ;
#15112 = CARTESIAN_POINT ( 'NONE',  ( 0.2967562270154266435, 4.638299250765053117, 0.09806193730438493572 ) ) ;
#15113 = B_SPLINE_CURVE_WITH_KNOTS ( 'NONE', 3,
 ( #5543, #1885, #2010, #7495, #1763, #18594, #11400, #16881, #18712, #172, #18832, #22362, #2127, #49, #5665, #14828, #17000, #10923 ),
 .UNSPECIFIED., .F., .F.,
 ( 4, 2, 2, 2, 2, 2, 2, 2, 4 ),
 ( 0.8132388816940862020, 0.8155224221455371625, 0.8178059625969880120, 0.8200895030484388615, 0.8223730434998898220, 0.8246565839513406715, 0.8269401244027916320, 0.8292236648542425925, 0.8315072053056934420 ),
 .UNSPECIFIED. ) ;
#15114 = CARTESIAN_POINT ( 'NONE',  ( -0.1954553509668046918, -0.1954553509668046640, 0.3730555555555596925 ) ) ;
#15115 = VECTOR ( 'NONE', #12290, 39.37007874015748854 ) ;
#15116 = LINE ( 'NONE', #21191, #20076 ) ;
#15117 = CYLINDRICAL_SURFACE ( 'NONE', #5833, 0.3125000000000000000 ) ;
#15118 = ORIENTED_EDGE ( 'NONE', *, *, #3928, .T. ) ;
#15119 = CARTESIAN_POINT ( 'NONE',  ( -0.1116596296178199582, 0.1758928570453147100, -0.3436530038418508792 ) ) ;
#15120 = CARTESIAN_POINT ( 'NONE',  ( -0.1993543840281267465, 0.5145833332574667462, 0.1993543840281266633 ) ) ;
#15121 = CARTESIAN_POINT ( 'NONE',  ( 0.000000000000000000, 0.01999999999999951469, 0.000000000000000000 ) ) ;
#15122 = CARTESIAN_POINT ( 'NONE',  ( 0.3149902191487801151, 0.4934499048855510717, -1.115388133222527722 ) ) ;
#15123 = DIRECTION ( 'NONE',  ( 0.4999999999999912292, -2.725147086360871558E-18, -0.8660254037844437036 ) ) ;
#15124 = CARTESIAN_POINT ( 'NONE',  ( 0.1954553509668046640, -0.1954553509668047195, 0.1716666666666691599 ) ) ;
#15125 = CARTESIAN_POINT ( 'NONE',  ( -0.3098116448389192645, 5.104813878284599760, -0.02126393433258285878 ) ) ;
#15126 = CARTESIAN_POINT ( 'NONE',  ( 0.4687500000000002776, 0.08844770643847373048, 0.4134734246479533359 ) ) ;
#15127 = CARTESIAN_POINT ( 'NONE',  ( -0.2206173157302028787, 0.2749999999999996891, 0.2206173157302027954 ) ) ;
#15128 = CARTESIAN_POINT ( 'NONE',  ( 0.3119999999999999996, 5.241749999999997911, 0.1292346314604056190 ) ) ;
#15129 = CARTESIAN_POINT ( 'NONE',  ( -0.2819296736111110424, 4.252166666742533074, -0.1167790944451423119 ) ) ;
#15130 = CARTESIAN_POINT ( 'NONE',  ( -0.1292346314604032043, 3.818138888888887639, -0.3120000000000024420 ) ) ;
#15131 = DIRECTION ( 'NONE',  ( -1.000000000000000000, -0.000000000000000000, -0.000000000000000000 ) ) ;
#15132 = EDGE_CURVE ( 'NONE', #1686, #21793, #1190, .T. ) ;
#15133 = EDGE_LOOP ( 'NONE', ( #1570, #14769 ) ) ;
#15134 = EDGE_CURVE ( 'NONE', #14458, #10194, #3335, .T. ) ;
#15135 = VECTOR ( 'NONE', #21688, 39.37007874015748143 ) ;
#15136 = CARTESIAN_POINT ( 'NONE',  ( -0.1167790944451423257, 4.898000000075866112, -0.2819296736111110424 ) ) ;
#15137 = DIRECTION ( 'NONE',  ( -0.000000000000000000, 1.000000000000000000, -0.000000000000000000 ) ) ;
#15138 = ADVANCED_FACE ( 'NONE', ( #712 ), #8140, .T. ) ;
#15139 = DIRECTION ( 'NONE',  ( 1.000000000000000000, 0.000000000000000000, 0.000000000000000000 ) ) ;
#15140 = CARTESIAN_POINT ( 'NONE',  ( 2.824051777240061223E-14, 3.849388889040854522, 0.3119999999999999996 ) ) ;
#15141 = CARTESIAN_POINT ( 'NONE',  ( -0.2819296736111110424, 4.578555555631421470, 0.1167790944451424923 ) ) ;
#15142 = CARTESIAN_POINT ( 'NONE',  ( -0.002064217775335610086, 4.043888859528191659, -0.3119941523652927096 ) ) ;
#15143 = CARTESIAN_POINT ( 'NONE',  ( -0.2764156081756484196, 1.692557448933383907E-17, 0.09527777777777970969 ) ) ;
#15144 = CARTESIAN_POINT ( 'NONE',  ( 0.1993543840281266910, 0.4451388888130222710, -0.1993543840281266910 ) ) ;
#15146 = VERTEX_POINT ( 'NONE', #23014 ) ;
#15145 = VECTOR ( 'NONE', #7377, 39.37007874015748143 ) ;
#15147 = CARTESIAN_POINT ( 'NONE',  ( -5.178964085587577574E-17, 0.5354166665908000056, 0.2819296736111110979 ) ) ;
#15148 = PLANE ( 'NONE',  #22060 ) ;
#15149 = CARTESIAN_POINT ( 'NONE',  ( -0.2472135954999579999, 0.008928571233486629066, 0.3402603233408160732 ) ) ;
#15150 = CARTESIAN_POINT ( 'NONE',  ( -0.3999999999999999667, 0.1464285714285713802, -0.1299678784931626030 ) ) ;
#15151 = CARTESIAN_POINT ( 'NONE',  ( 0.1306872919485616846, 0.3155070326520292290, 0.1560416666666688823 ) ) ;
#15152 = CARTESIAN_POINT ( 'NONE',  ( -1.322549964794167179E-16, 0.7885332705621128646, -1.079944001585411595 ) ) ;
#15153 = CARTESIAN_POINT ( 'NONE',  ( -0.2728104005625175965, -0.05992465826476112839, -0.06807390018913435370 ) ) ;
#15154 = CARTESIAN_POINT ( 'NONE',  ( -0.1167790944451424506, 0.2958333332574667462, 0.2819296736111110424 ) ) ;
#15155 = CARTESIAN_POINT ( 'NONE',  ( 0.2819296736111110424, 0.3097222221463555303, 0.1167790944451424923 ) ) ;
#15156 = CARTESIAN_POINT ( 'NONE',  ( -0.1167790944451423257, 4.245222222298088433, -0.2819296736111110424 ) ) ;
#15157 = CARTESIAN_POINT ( 'NONE',  ( 0.3999999999999999667, 0.1732142855192008724, 0.1299678784931626307 ) ) ;
#15158 = CARTESIAN_POINT ( 'NONE',  ( -0.1167790944451423257, 4.967444444520310753, -0.2819296736111110424 ) ) ;
#15159 = CARTESIAN_POINT ( 'NONE',  ( -1.726321361862525858E-17, 4.338972222298087544, -0.2819296736111110979 ) ) ;
#15160 = FACE_OUTER_BOUND ( 'NONE', #8929, .T. ) ;
#15161 = ORIENTED_EDGE ( 'NONE', *, *, #14895, .F. ) ;
#15162 = CARTESIAN_POINT ( 'NONE',  ( 0.4805070082343983473, -0.2560807851245830435, 0.04413116910601658921 ) ) ;
#15163 = CARTESIAN_POINT ( 'NONE',  ( 0.3119999999999999996, 4.033416666818398610, -0.1292346314604056745 ) ) ;
#15164 = CARTESIAN_POINT ( 'NONE',  ( 0.000000000000000000, 0.8699999999999998845, -0.2109499999999998043 ) ) ;
#15165 = VECTOR ( 'NONE', #23440, 39.37007874015748143 ) ;
#15166 = CARTESIAN_POINT ( 'NONE',  ( 0.3950000000000000178, 2.665000000000000036, -2.540999999999999925 ) ) ;
#15167 = ORIENTED_EDGE ( 'NONE', *, *, #16032, .F. ) ;
#15168 = PERSON_AND_ORGANIZATION_ROLE ( 'classification_officer' ) ;
#15169 = DIRECTION ( 'NONE',  ( 0.000000000000000000, 0.000000000000000000, -1.000000000000000000 ) ) ;
#15170 = DIRECTION ( 'NONE',  ( 0.3993784937532309232, -0.7060941387255963431, -0.5847460012558945985 ) ) ;
#15171 = CARTESIAN_POINT ( 'NONE',  ( -0.08124123436041086332, 4.990575526692240693, -0.3039879947993704423 ) ) ;
#15172 = ORIENTED_EDGE ( 'NONE', *, *, #19009, .F. ) ;
#15173 = CARTESIAN_POINT ( 'NONE',  ( 0.3119999999999998885, 0.4520833331816004885, 0.1292346314604058410 ) ) ;
#15174 = EDGE_LOOP ( 'NONE', ( #13241, #7546, #18595, #22506 ) ) ;
#15175 = DIRECTION ( 'NONE',  ( -0.000000000000000000, -1.000000000000000000, -0.000000000000000000 ) ) ;
#15176 = CARTESIAN_POINT ( 'NONE',  ( 0.1893589898698054830, 0.4210708385985185154, 0.4333520680959464522 ) ) ;
#15177 = CARTESIAN_POINT ( 'NONE',  ( 0.0003672435171428997994, 4.766045129345851450, -0.3119998398083521085 ) ) ;
#15178 = CARTESIAN_POINT ( 'NONE',  ( -0.2233192592356399442, 0.01874999990245759460, -0.3073725909049500049 ) ) ;
#15179 = FACE_OUTER_BOUND ( 'NONE', #16131, .T. ) ;
#15180 = CARTESIAN_POINT ( 'NONE',  ( 0.2923287055106771337, 0.1473214284738861568, 0.2123892367102621359 ) ) ;
#15181 = AXIS2_PLACEMENT_3D ( 'NONE', #13049, #14625, #1571 ) ;
#15182 = LINE ( 'NONE', #15423, #16594 ) ;
#15183 = CARTESIAN_POINT ( 'NONE',  ( 0.1954553509668047195, 0.1954553509668046085, 0.4008333333333377047 ) ) ;
#15184 = CARTESIAN_POINT ( 'NONE',  ( -0.2819296736111110424, 3.904944444520309865, -0.1167790944451423119 ) ) ;
#15185 = CARTESIAN_POINT ( 'NONE',  ( -0.1557525356064938249, -0.4513421090059194229, 0.4242370903633182477 ) ) ;
#15186 = CARTESIAN_POINT ( 'NONE',  ( -0.05485615681475838196, 0.5228774440028900461, 0.05347937985141015815 ) ) ;
#15187 = CARTESIAN_POINT ( 'NONE',  ( -0.3119999999999999996, 3.769527777777778255, -0.1292346314604056468 ) ) ;
#15188 = CARTESIAN_POINT ( 'NONE',  ( 0.2206173157302027954, 4.814666666818398610, -0.2206173157302028232 ) ) ;
#15189 = CARTESIAN_POINT ( 'NONE',  ( 0.2819296736111110979, 5.005638888964754507, -3.452642723725051716E-17 ) ) ;
#15190 = EDGE_LOOP ( 'NONE', ( #24072, #22072, #16182, #168 ) ) ;
#15191 = CARTESIAN_POINT ( 'NONE',  ( -0.1167790944451423535, 4.307722222298088433, 0.2819296736111110424 ) ) ;
#15192 = ORIENTED_EDGE ( 'NONE', *, *, #20114, .F. ) ;
#15193 = CARTESIAN_POINT ( 'NONE',  ( -6.979263641208234666E-17, 0.1187499999024575897, 0.3799334167787516980 ) ) ;
#15194 = ORIENTED_EDGE ( 'NONE', *, *, #11117, .T. ) ;
#15195 = VECTOR ( 'NONE', #23666, 39.37007874015748143 ) ;
#15196 = CIRCLE ( 'NONE', #778, 0.2499999999999999722 ) ;
#15197 = ORIENTED_EDGE ( 'NONE', *, *, #14848, .T. ) ;
#15198 = PERSON_AND_ORGANIZATION_ROLE ( 'creator' ) ;
#15199 = CARTESIAN_POINT ( 'NONE',  ( 0.2977100099089716734, 3.659999999999999698, -0.09499999999999995948 ) ) ;
#15200 = CARTESIAN_POINT ( 'NONE',  ( -0.1993543840281266355, 5.193138888964753619, 0.1993543840281267465 ) ) ;
#15201 = CARTESIAN_POINT ( 'NONE',  ( 0.2819296736111111534, 3.946611111186976828, 0.1167790944451422563 ) ) ;
#15202 = CARTESIAN_POINT ( 'NONE',  ( 0.1079706958816955137, 4.429610341295819431, -0.2927247107414157612 ) ) ;
#15203 = CARTESIAN_POINT ( 'NONE',  ( -3.385114897866767815E-17, -0.2764156081756484196, 0.3313888888888926743 ) ) ;
#15204 = CARTESIAN_POINT ( 'NONE',  ( 0.3886563986011730143, -0.3298860868734675433, 0.06108838700205718175 ) ) ;
#15205 = ORIENTED_EDGE ( 'NONE', *, *, #20996, .T. ) ;
#15206 = CARTESIAN_POINT ( 'NONE',  ( 0.1144950937579611444, 0.2764156081756483641, 0.3487500000000039457 ) ) ;
#15207 = CARTESIAN_POINT ( 'NONE',  ( 0.2819296736111110979, 0.4381944443685778512, 0.000000000000000000 ) ) ;
#15208 = CARTESIAN_POINT ( 'NONE',  ( 0.000000000000000000, 0.2764156081756484196, -0.1477777777777777857 ) ) ;
#15209 = CARTESIAN_POINT ( 'NONE',  ( 0.2819296736111110979, 5.061194444520310753, -3.452642723725051716E-17 ) ) ;
#15210 = CARTESIAN_POINT ( 'NONE',  ( -0.008438385721254092545, -0.5369265497013727684, 0.04763613967036315483 ) ) ;
#15211 = CARTESIAN_POINT ( 'NONE',  ( -0.1167790944451423257, 4.564666666742531298, -0.2819296736111110424 ) ) ;
#15212 = CARTESIAN_POINT ( 'NONE',  ( -0.2631830812676746456, 0.1021974198356742081, -0.07133656933612833595 ) ) ;
#15213 =( BOUNDED_SURFACE ( )  B_SPLINE_SURFACE ( 3, 2, ( 
 ( #6545, #10343, #13996 ),
 ( #21426, #4714, #21543 ),
 ( #19118, #2423, #9864 ),
 ( #17292, #21067, #18343 ),
 ( #20296, #23810, #16873 ),
 ( #12880, #11155, #16402 ) ),
 .UNSPECIFIED., .F., .F., .F. ) 
 B_SPLINE_SURFACE_WITH_KNOTS ( ( 4, 2, 4 ),
 ( 3, 3 ),
 ( 0.001022076388580720786, 0.001521441877679464375, 0.002020807366778207964 ),
 ( 0.000000000000000000, 1.000000000000000000 ),
 .UNSPECIFIED. ) 
 GEOMETRIC_REPRESENTATION_ITEM ( )  RATIONAL_B_SPLINE_SURFACE ( (
 ( 1.000000000000000000, 0.8285407536241365944, 1.000000000000000000),
 ( 1.000000000000000000, 0.8382697314792307841, 1.000000000000000000),
 ( 1.000000000000000000, 0.8433836253084445733, 1.000000000000000000),
 ( 1.000000000000000000, 0.8433992480894338950, 1.000000000000000000),
 ( 1.000000000000000000, 0.8382827608170095868, 1.000000000000000000),
 ( 1.000000000000000000, 0.8285407536241039539, 1.000000000000000000) ) ) 
 REPRESENTATION_ITEM ( '' )  SURFACE ( )  );
#15214 = VECTOR ( 'NONE', #14744, 39.37007874015748143 ) ;
#15215 = DIRECTION ( 'NONE',  ( -0.8660254037844377084, 0.000000000000000000, 0.5000000000000015543 ) ) ;
#15216 = DIRECTION ( 'NONE',  ( 1.000000000000000000, 0.000000000000000000, 0.000000000000000000 ) ) ;
#15217 = CARTESIAN_POINT ( 'NONE',  ( 1.711101542529408048, 2.439517176785165109, -2.020270991558039242 ) ) ;
#15218 = B_SPLINE_CURVE_WITH_KNOTS ( 'NONE', 3,
 ( #8489, #15931, #4829, #12299 ),
 .UNSPECIFIED., .F., .F.,
 ( 4, 4 ),
 ( 0.02432858112762280312, 0.08935694927272851140 ),
 .UNSPECIFIED. ) ;
#15219 = CARTESIAN_POINT ( 'NONE',  ( -0.2206173157302027676, 4.613277777777776478, 0.2206173157302028787 ) ) ;
#15220 = VECTOR ( 'NONE', #15123, 39.37007874015748143 ) ;
#15221 = CARTESIAN_POINT ( 'NONE',  ( -0.2819296736111110424, 3.745222222298088433, 0.1167790944451424923 ) ) ;
#15222 = CARTESIAN_POINT ( 'NONE',  ( 1.910449006669871087E-17, 0.3583333331816003775, -0.3119999999999999996 ) ) ;
#15223 = CARTESIAN_POINT ( 'NONE',  ( 1.020000000000000018, 0.05000000000000028727, -2.591000000000000192 ) ) ;
#15224 = APPROVAL ( #11910, 'UNSPECIFIED' ) ;
#15225 = ORIENTED_EDGE ( 'NONE', *, *, #21301, .F. ) ;
#15226 = CYLINDRICAL_SURFACE ( 'NONE', #11285, 0.3119999999999999996 ) ;
#15227 = EDGE_LOOP ( 'NONE', ( #13094, #2746 ) ) ;
#15228 = CARTESIAN_POINT ( 'NONE',  ( -0.1964672255785171739, -0.4278354717905788474, 0.4172182224143143880 ) ) ;
#15229 = CARTESIAN_POINT ( 'NONE',  ( 0.04602711923241634834, 4.628539372138874342, 0.3120000069469925363 ) ) ;
#15230 = CARTESIAN_POINT ( 'NONE',  ( -0.1954553509668046640, 0.1954553509668046918, 0.4702777777777827350 ) ) ;
#15231 = VECTOR ( 'NONE', #7576, 39.37007874015748143 ) ;
#15232 = CARTESIAN_POINT ( 'NONE',  ( 0.1569173507168480086, 4.298453709044838256, 0.2727343952408894379 ) ) ;
#15233 = ORIENTED_EDGE ( 'NONE', *, *, #7092, .F. ) ;
#15234 = CARTESIAN_POINT ( 'NONE',  ( 2.326421213736078119E-17, 0.08303571418817184968, -0.3799334167787516425 ) ) ;
#15235 = CARTESIAN_POINT ( 'NONE',  ( 0.1167790944451423257, 0.5458333332574666352, -0.2819296736111110424 ) ) ;
#15236 = CARTESIAN_POINT ( 'NONE',  ( -0.2082794372640225100, 5.206640035683668621, 0.1900105704308308607 ) ) ;
#15237 = CARTESIAN_POINT ( 'NONE',  ( 0.04147192196593674912, 0.7863862574794888705, -1.079910930672920655 ) ) ;
#15238 = LINE ( 'NONE', #22667, #8596 ) ;
#15239 = CARTESIAN_POINT ( 'NONE',  ( 0.2764156081756483641, -0.1144950937579611167, 0.1195833333333354426 ) ) ;
#15240 = DIRECTION ( 'NONE',  ( 1.224646799147353207E-16, 0.000000000000000000, -1.000000000000000000 ) ) ;
#15241 = CARTESIAN_POINT ( 'NONE',  ( -0.2206173157302028787, 0.2194444444444441089, 0.2206173157302027954 ) ) ;
#15242 = CARTESIAN_POINT ( 'NONE',  ( 0.3119999999999999996, 5.186194444444442553, 0.1292346314604056190 ) ) ;
#15243 = EDGE_CURVE ( 'NONE', #11248, #19113, #470, .T. ) ;
#15244 = CARTESIAN_POINT ( 'NONE',  ( -0.1167790944451423257, 4.134111111186977716, -0.2819296736111110424 ) ) ;
#15245 = CARTESIAN_POINT ( 'NONE',  ( -0.1917964032624795701, 4.327441163112869305, -0.2494539190351865721 ) ) ;
#15246 = LINE ( 'NONE', #11144, #17179 ) ;
#15247 = DIRECTION ( 'NONE',  ( 0.000000000000000000, 0.000000000000000000, -1.000000000000000000 ) ) ;
#15248 = CARTESIAN_POINT ( 'NONE',  ( 0.2209708691207961095, -0.2209708691207961651, 0.1438888888888913697 ) ) ;
#15249 = CARTESIAN_POINT ( 'NONE',  ( -0.1167790944451423535, 4.918833333409199149, 0.2819296736111110424 ) ) ;
#15250 = CARTESIAN_POINT ( 'NONE',  ( 0.05483022876054116646, 0.5228926224321454042, 0.05347271648848982151 ) ) ;
#15251 = CARTESIAN_POINT ( 'NONE',  ( -0.009801821498707709301, 5.143598273731186943, -0.3039077880706267942 ) ) ;
#15252 =( BOUNDED_CURVE ( )  B_SPLINE_CURVE ( 2, ( #253, #22568, #6096, #491, #616, #11725, #735, #8046, #18788 ),
 .UNSPECIFIED., .F., .T. ) 
 B_SPLINE_CURVE_WITH_KNOTS ( ( 3, 2, 2, 2, 3 ),
 ( 0.8958333333333333703, 0.9062500000000000000, 0.9166666666666666297, 0.9270833333333333703, 0.9375000000000000000 ),
 .UNSPECIFIED. ) 
 CURVE ( )  GEOMETRIC_REPRESENTATION_ITEM ( )  RATIONAL_B_SPLINE_CURVE ( ( 1.000000000000000000, 0.9238795325112867385, 1.000000000000000000, 0.9238795325112867385, 1.000000000000000000, 0.9238795325112867385, 1.000000000000000000, 0.9238795325112867385, 1.000000000000000000 ) ) 
 REPRESENTATION_ITEM ( '' )  );
#15253 = DIRECTION ( 'NONE',  ( -0.2060615672115666819, 0.9523468275765514246, 0.2248869727734167101 ) ) ;
#15254 = CARTESIAN_POINT ( 'NONE',  ( 0.0005601723535045452463, 3.710484947398785316, -0.3119995287117768856 ) ) ;
#15255 = CARTESIAN_POINT ( 'NONE',  ( 0.2764156081756484196, -5.077672346800151106E-17, -0.1061111111111107813 ) ) ;
#15256 = CARTESIAN_POINT ( 'NONE',  ( -0.1993543840281266910, 4.359805555631421470, -0.1993543840281266910 ) ) ;
#15257 = CONTEXT_DEPENDENT_SHAPE_REPRESENTATION ( #2203, #20254 ) ;
#15258 = ORIENTED_EDGE ( 'NONE', *, *, #13809, .T. ) ;
#15259 = CARTESIAN_POINT ( 'NONE',  ( -0.1999482914134789180, 4.050008517921297013, -0.2395145290917104208 ) ) ;
#15260 = CARTESIAN_POINT ( 'NONE',  ( 0.1954553509668047195, 0.1954553509668046085, 0.01888888888889020401 ) ) ;
#15261 = B_SPLINE_CURVE_WITH_KNOTS ( 'NONE', 3,
 ( #21530, #15921, #14220, #4818, #3122, #4944, #13987, #23225, #14102, #6534, #8479, #23467, #21657, #12408, #811, #10573, #23344, #6655, #21414, #17758, #12171, #12288, #19827, #2646, #19579, #6415, #15692, #13869, #2872, #16052, #17881, #10095, #10331, #3005, #12049, #1173, #21296, #8611, #4590, #6777, #17516, #19462, #17637, #926 ),
 .UNSPECIFIED., .F., .F.,
 ( 4, 2, 2, 2, 2, 2, 2, 2, 2, 2, 2, 2, 2, 2, 2, 2, 2, 2, 2, 2, 2, 4 ),
 ( 0.03213067753877397320, 0.03370072127975529824, 0.03448574315024595383, 0.03527076502073661635, 0.03684080876171794139, 0.03762583063220859697, 0.03841085250269925255, 0.03998089624368057760, 0.04155093998466190264, 0.04233596185515256516, 0.04312098372564323462, 0.04469102746662455966, 0.04626107120760588470, 0.04783111494858721668, 0.04861613681907787921, 0.04940115868956854173, 0.05097120243054986677, 0.05254124617153120569, 0.05332626804202186821, 0.05411128991251254461, 0.05568133365349388353, 0.05725137739447521551 ),
 .UNSPECIFIED. ) ;
#15262 = CARTESIAN_POINT ( 'NONE',  ( 0.06335377612981453466, 0.2731694899447553726, -0.3999999999999999667 ) ) ;
#15263 = ADVANCED_FACE ( 'NONE', ( #4485 ), #20668, .F. ) ;
#15264 = ORIENTED_EDGE ( 'NONE', *, *, #59, .F. ) ;
#15265 = CARTESIAN_POINT ( 'NONE',  ( -0.2819296736111110979, 0.4138888888130222155, 0.1167790944451422425 ) ) ;
#15266 = FACE_OUTER_BOUND ( 'NONE', #10276, .T. ) ;
#15267 = CARTESIAN_POINT ( 'NONE',  ( -0.2209708691207961373, -0.2209708691207961095, 0.1786111111111135241 ) ) ;
#15268 = CARTESIAN_POINT ( 'NONE',  ( -0.2472135954999579444, 0.2107142857142856318, -0.3402603233408159622 ) ) ;
#15269 = CARTESIAN_POINT ( 'NONE',  ( 0.3155070326520292290, -0.1306872919485616569, 0.2532638888888918971 ) ) ;
#15270 = CARTESIAN_POINT ( 'NONE',  ( -0.1583529533612729467, -0.4498407571151714079, 0.08855978515309881338 ) ) ;
#15271 = CARTESIAN_POINT ( 'NONE',  ( 0.7919466436700954848, 2.740039370078740433, -2.986000000000000210 ) ) ;
#15272 = CARTESIAN_POINT ( 'NONE',  ( 0.1993543840281266910, 0.3756944443685777957, -0.1993543840281266910 ) ) ;
#15273 = CARTESIAN_POINT ( 'NONE',  ( -0.1167790944451422702, 0.3305555554796889561, -0.2819296736111110424 ) ) ;
#15274 = CARTESIAN_POINT ( 'NONE',  ( 0.2819296736111110424, 4.342444444520311642, -0.1167790944451423396 ) ) ;
#15275 = CARTESIAN_POINT ( 'NONE',  ( -0.3999999999999999667, 0.3517857140906293645, -0.1299678784931626030 ) ) ;
#15276 = EDGE_CURVE ( 'NONE', #2366, #10939, #17890, .T. ) ;
#15277 = CARTESIAN_POINT ( 'NONE',  ( 0.1993543840281267465, 4.887583333409199149, 0.1993543840281266633 ) ) ;
#15278 = CARTESIAN_POINT ( 'NONE',  ( -0.2819296736111110424, 4.134111111186976828, 0.1167790944451424923 ) ) ;
#15279 = LINE ( 'NONE', #15045, #18034 ) ;
#15280 = CARTESIAN_POINT ( 'NONE',  ( -0.05482159418620013297, 0.5228976771666257184, 0.05347049744907691332 ) ) ;
#15281 = CARTESIAN_POINT ( 'NONE',  ( 0.3119999999999999996, 4.137583333485066461, 0.1292346314604056190 ) ) ;
#15282 = CARTESIAN_POINT ( 'NONE',  ( 9.101228903679513089E-16, 0.3017857140906293756, 0.4000000000000000222 ) ) ;
#15283 = LINE ( 'NONE', #22599, #10700 ) ;
#15284 = ORIENTED_EDGE ( 'NONE', *, *, #10816, .T. ) ;
#15285 = APPROVAL_STATUS ( 'not_yet_approved' ) ;
#15286 = EDGE_LOOP ( 'NONE', ( #6033, #15640, #21608, #667 ) ) ;
#15287 = FACE_OUTER_BOUND ( 'NONE', #15316, .T. ) ;
#15288 = CARTESIAN_POINT ( 'NONE',  ( 0.000000000000000000, 5.384999999999999787, -0.3119999999999999996 ) ) ;
#15289 = CARTESIAN_POINT ( 'NONE',  ( -0.3058731308713533159, 5.000420509829539562, -0.06261731312025432816 ) ) ;
#15290 = ORIENTED_EDGE ( 'NONE', *, *, #1692, .T. ) ;
#15291 = CARTESIAN_POINT ( 'NONE',  ( 0.1292346314604057023, 0.4451388887371560688, 0.3119999999999998885 ) ) ;
#15292 = EDGE_CURVE ( 'NONE', #21037, #19685, #6251, .T. ) ;
#15293 = EDGE_CURVE ( 'NONE', #20467, #787, #22558, .T. ) ;
#15294 = ORIENTED_EDGE ( 'NONE', *, *, #17225, .F. ) ;
#15295 = LINE ( 'NONE', #6012, #22959 ) ;
#15296 = DIRECTION ( 'NONE',  ( -0.000000000000000000, -1.000000000000000000, -0.000000000000000000 ) ) ;
#15297 = CARTESIAN_POINT ( 'NONE',  ( -0.4749999999999999778, 3.575000000000000622, 0.09499999999999995948 ) ) ;
#15298 = CARTESIAN_POINT ( 'NONE',  ( 0.3613381517857143232, 0.06874999990245758696, -0.1174058825155740587 ) ) ;
#15299 = CARTESIAN_POINT ( 'NONE',  ( 0.1789513046941397512, 5.185541748123438488, -0.2296687052981416510 ) ) ;
#15300 = EDGE_LOOP ( 'NONE', ( #4158, #8099, #3898, #21089 ) ) ;
#15301 = CARTESIAN_POINT ( 'NONE',  ( -0.2923287055106771337, 0.4116071427596003640, 0.2123892367102619971 ) ) ;
#15302 = DIRECTION ( 'NONE',  ( 0.000000000000000000, 0.000000000000000000, -1.000000000000000000 ) ) ;
#15303 = CARTESIAN_POINT ( 'NONE',  ( -0.2447627460273846534, 4.674789551421016043, 0.1936577326920176922 ) ) ;
#15304 = EDGE_CURVE ( 'NONE', #4460, #12631, #21385, .T. ) ;
#15305 = CARTESIAN_POINT ( 'NONE',  ( -0.1993543840281266355, 3.970916666742532186, 0.1993543840281267465 ) ) ;
#15306 = CARTESIAN_POINT ( 'NONE',  ( -0.4224645524279253550, -0.2973558542979372055, 0.3902541392329982317 ) ) ;
#15307 = CARTESIAN_POINT ( 'NONE',  ( -0.1653103785569667583, 0.4584405057248003845, 0.07159583130656674288 ) ) ;
#15308 = CARTESIAN_POINT ( 'NONE',  ( -0.1940754166076595899, 5.189177002903242020, 0.2157554602168622049 ) ) ;
#15309 = CARTESIAN_POINT ( 'NONE',  ( 0.3119999999999999996, 4.644527777929510215, -0.1292346314604056745 ) ) ;
#15310 = CONICAL_SURFACE ( 'NONE', #14929, 0.2500000000000000555, 0.5235987755985997971 ) ;
#15311 = CARTESIAN_POINT ( 'NONE',  ( -0.2819296736111110979, 5.029944444520308977, -0.1167790944451422980 ) ) ;
#15312 = ORIENTED_EDGE ( 'NONE', *, *, #6373, .F. ) ;
#15313 = CARTESIAN_POINT ( 'NONE',  ( -1.726321361862525858E-17, 4.338972222298087544, -0.2819296736111110979 ) ) ;
#15314 = CARTESIAN_POINT ( 'NONE',  ( -0.1116596296178200276, 0.1151785713310290032, 0.3436530038418508792 ) ) ;
#15315 = EDGE_CURVE ( 'NONE', #18304, #4025, #17895, .T. ) ;
#15316 = EDGE_LOOP ( 'NONE', ( #18780, #1166, #12058, #22600 ) ) ;
#15317 = ORIENTED_EDGE ( 'NONE', *, *, #2636, .T. ) ;
#15318 = APPROVAL_DATE_TIME ( #21039, #9095 ) ;
#15319 = FACE_OUTER_BOUND ( 'NONE', #3518, .T. ) ;
#15320 = CARTESIAN_POINT ( 'NONE',  ( 0.1167790944451422702, 3.904944444520310309, -0.2819296736111110979 ) ) ;
#15321 = CONICAL_SURFACE ( 'NONE', #9880, 0.2041999999999999926, 0.7853981633974563836 ) ;
#15322 = CARTESIAN_POINT ( 'NONE',  ( 0.2450693591352816059, 4.424882274230782286, -0.1965390533656376226 ) ) ;
#15323 = CARTESIAN_POINT ( 'NONE',  ( 0.3119999999999999996, 4.634111111111110404, -3.820898013339742174E-17 ) ) ;
#15324 = CARTESIAN_POINT ( 'NONE',  ( 1.149903810567666440, 2.740000000000000213, -2.516000000000000014 ) ) ;
#15325 = CARTESIAN_POINT ( 'NONE',  ( -0.2764156081756484196, 0.1144950937579609918, 0.1404166666666689656 ) ) ;
#15326 = CARTESIAN_POINT ( 'NONE',  ( -0.2819296736111111534, 0.5805555554796888451, 0.1167790944451422563 ) ) ;
#15327 = CARTESIAN_POINT ( 'NONE',  ( 0.2764156081756483641, -0.1144950937579611167, -0.1095833333333330328 ) ) ;
#15328 = ADVANCED_FACE ( 'NONE', ( #2971 ), #4917, .T. ) ;
#15329 = EDGE_LOOP ( 'NONE', ( #4549, #2076, #7438, #20134 ) ) ;
#15330 = CARTESIAN_POINT ( 'NONE',  ( 0.2819296736111110979, 4.668833333409200037, 0.1167790944451422425 ) ) ;
#15331 = CARTESIAN_POINT ( 'NONE',  ( -0.006464354918053499821, -0.5491938321437417336, 0.04193567535760733128 ) ) ;
#15332 = EDGE_CURVE ( 'NONE', #20123, #1661, #23198, .T. ) ;
#15333 = CARTESIAN_POINT ( 'NONE',  ( 0.1167790944451424368, 4.648000000075865223, 0.2819296736111110424 ) ) ;
#15334 = CARTESIAN_POINT ( 'NONE',  ( -0.0001107979596245131973, 4.154947627944543420, -0.3120000001382827182 ) ) ;
#15335 = CARTESIAN_POINT ( 'NONE',  ( 1.522235971340160240E-16, 0.01999999999999951469, -1.243000000000000105 ) ) ;
#15336 = LINE ( 'NONE', #570, #2819 ) ;
#15337 = PLANE ( 'NONE',  #1835 ) ;
#15338 = CARTESIAN_POINT ( 'NONE',  ( -1.910449006669871087E-17, 4.481333333333331836, -0.3119999999999999996 ) ) ;
#15339 = CARTESIAN_POINT ( 'NONE',  ( -0.06335377612981449302, 0.2768305100552443943, -0.4000000000000000222 ) ) ;
#15340 = CARTESIAN_POINT ( 'NONE',  ( 0.009374999999999772404, 0.5358532185916217161, 0.3779506566538943790 ) ) ;
#15341 = VERTEX_POINT ( 'NONE', #1265 ) ;
#15342 = CARTESIAN_POINT ( 'NONE',  ( 9.065143943205062133E-18, 0.05000000000000028727, -2.194053356329904947 ) ) ;
#15343 = ORIENTED_EDGE ( 'NONE', *, *, #3784, .F. ) ;
#15344 = AXIS2_PLACEMENT_3D ( 'NONE', #13803, #21112, #21472 ) ;
#15345 = CARTESIAN_POINT ( 'NONE',  ( 0.2761937380445508849, 4.700912946670643855, -0.1452742419101630544 ) ) ;
#15346 = CARTESIAN_POINT ( 'NONE',  ( 0.1171198219552221365, 4.651519741485643955, -0.2900815769309791348 ) ) ;
#15347 = CARTESIAN_POINT ( 'NONE',  ( 0.2764156081756483641, -0.1144950937579611167, 0.3904166666666709085 ) ) ;
#15348 = CARTESIAN_POINT ( 'NONE',  ( 1.573500000000000343, -3.414809992080329023E-17, -0.5649999999999999467 ) ) ;
#15349 = EDGE_LOOP ( 'NONE', ( #10281, #10559, #20797, #13949 ) ) ;
#15350 =( BOUNDED_CURVE ( )  B_SPLINE_CURVE ( 2, ( #10672, #1402, #8707, #16158, #8830, #6886, #12273, #14329, #23690 ),
 .UNSPECIFIED., .F., .F. ) 
 B_SPLINE_CURVE_WITH_KNOTS ( ( 3, 2, 2, 2, 3 ),
 ( 0.2812500000000000555, 0.2916666666666667407, 0.3020833333333333703, 0.3125000000000000000, 0.3229166666666666852 ),
 .UNSPECIFIED. ) 
 CURVE ( )  GEOMETRIC_REPRESENTATION_ITEM ( )  RATIONAL_B_SPLINE_CURVE ( ( 0.9999999999999995559, 0.9238795325112871826, 1.000000000000000000, 0.9238795325112867385, 1.000000000000000000, 0.9238795325112867385, 1.000000000000000000, 0.9238795325112871826, 0.9999999999999995559 ) ) 
 REPRESENTATION_ITEM ( '' )  );
#15351 = CARTESIAN_POINT ( 'NONE',  ( 0.3613381517857143232, -0.006250000097542392913, 0.000000000000000000 ) ) ;
#15352 = CARTESIAN_POINT ( 'NONE',  ( 0.1993543840281266910, 0.3756944443685777957, -0.1993543840281266910 ) ) ;
#15353 = CARTESIAN_POINT ( 'NONE',  ( -0.1144950937579609779, 0.2764156081756484196, -0.1373611111111110450 ) ) ;
#15354 = CARTESIAN_POINT ( 'NONE',  ( 0.1018054737164394014, 0.1946304594345829864, -1.235041780627553987 ) ) ;
#15355 = CARTESIAN_POINT ( 'NONE',  ( -5.731347020009612645E-17, 0.3861111109593781676, 0.3119999999999999996 ) ) ;
#15356 = CARTESIAN_POINT ( 'NONE',  ( 0.2764156081756483641, -0.1144950937579611167, 0.2306944444444474218 ) ) ;
#15357 = VECTOR ( 'NONE', #19347, 39.37007874015748143 ) ;
#15358 = CARTESIAN_POINT ( 'NONE',  ( -0.2917190787933745533, 4.609974286260102971, -0.1140841330618171251 ) ) ;
#15359 = CARTESIAN_POINT ( 'NONE',  ( 0.3999999999999999667, 0.1089285712334865930, -0.1299678784931625197 ) ) ;
#15360 = CARTESIAN_POINT ( 'NONE',  ( -0.3039006371514270666, -1.707404996040164820E-17, -0.2596894543520890108 ) ) ;
#15361 = CARTESIAN_POINT ( 'NONE',  ( -0.1292346314604058410, 0.1673611111111107941, 0.3119999999999998885 ) ) ;
#15362 = CARTESIAN_POINT ( 'NONE',  ( -0.2206173157302027676, 5.168833333333332725, 0.2206173157302028787 ) ) ;
#15363 = CARTESIAN_POINT ( 'NONE',  ( 0.2819296736111110979, 4.283416666742533074, -3.452642723725051716E-17 ) ) ;
#15364 = CARTESIAN_POINT ( 'NONE',  ( 5.731347020009612645E-17, 3.842444444444443441, 0.3119999999999999996 ) ) ;
#15365 = DIRECTION ( 'NONE',  ( -0.8651979924482607887, 0.04370253788966922681, 0.4995222938423283243 ) ) ;
#15366 = LINE ( 'NONE', #22795, #14948 ) ;
#15367 = VECTOR ( 'NONE', #22320, 39.37007874015748143 ) ;
#15368 = EDGE_LOOP ( 'NONE', ( #8844, #17395, #19115, #18541 ) ) ;
#15369 = VERTEX_POINT ( 'NONE', #11899 ) ;
#15370 = DIRECTION ( 'NONE',  ( 0.000000000000000000, 0.000000000000000000, 1.000000000000000000 ) ) ;
#15371 = CARTESIAN_POINT ( 'NONE',  ( 0.1993543840281266633, 4.720916666742532186, -0.1993543840281266910 ) ) ;
#15372 = CARTESIAN_POINT ( 'NONE',  ( -0.2233192592356400275, 0.3258928570453145102, 0.3073725909049499494 ) ) ;
#15373 = ADVANCED_FACE ( 'NONE', ( #19317 ), #2842, .F. ) ;
#15374 = CARTESIAN_POINT ( 'NONE',  ( -1.910449006669871087E-17, 4.092444444444444329, -0.3119999999999999996 ) ) ;
#15375 = ADVANCED_FACE ( 'NONE', ( #8451 ), #3998, .T. ) ;
#15376 = DIRECTION ( 'NONE',  ( 0.2851880286125162978, -0.1613946154526426924, 0.9447854605353536162 ) ) ;
#15377 = FACE_OUTER_BOUND ( 'NONE', #23570, .T. ) ;
#15378 = CARTESIAN_POINT ( 'NONE',  ( -0.2819296736111110979, 4.422305555631421470, 0.000000000000000000 ) ) ;
#15379 = CALENDAR_DATE ( 2026, 7, 10 ) ;
#15380 = CC_DESIGN_PERSON_AND_ORGANIZATION_ASSIGNMENT ( #13235, #15168, ( #2926 ) ) ;
#15381 = CARTESIAN_POINT ( 'NONE',  ( -0.3080870731862870859, 4.059453030256765516, 0.06306296359780783067 ) ) ;
#15382 = CARTESIAN_POINT ( 'NONE',  ( -0.2764156081756484196, 0.1144950937579609918, 0.09180555555555744429 ) ) ;
#15383 = LOCAL_TIME ( 21, 9, 13.00000000000000000, #17147 ) ;
#15384 = CARTESIAN_POINT ( 'NONE',  ( 0.3613381517857143232, -0.05982142866897096484, 0.000000000000000000 ) ) ;
#15385 = CARTESIAN_POINT ( 'NONE',  ( 0.1167790944451423257, 0.5041666665908002276, -0.2819296736111110424 ) ) ;
#15386 = DIRECTION ( 'NONE',  ( -1.000000000000000000, 0.000000000000000000, 0.000000000000000000 ) ) ;
#15387 = DIRECTION ( 'NONE',  ( -0.000000000000000000, -1.000000000000000000, -0.000000000000000000 ) ) ;
#15388 = CARTESIAN_POINT ( 'NONE',  ( 0.1236067977499789028, 0.09999999999999997780, 0.3804226065180614791 ) ) ;
#15389 = CARTESIAN_POINT ( 'NONE',  ( 0.3155070326520292290, 0.1306872919485615736, 0.1490972222222243793 ) ) ;
#15390 = CARTESIAN_POINT ( 'NONE',  ( 0.1292346314604058410, 3.957027777777776922, 0.3119999999999998885 ) ) ;
#15391 = CARTESIAN_POINT ( 'NONE',  ( -0.2798077087188347578, -0.01523944824431633545, -0.06897437538550148239 ) ) ;
#15392 = CARTESIAN_POINT ( 'NONE',  ( 0.2819296736111110979, 0.5909722221463555858, 0.000000000000000000 ) ) ;
#15393 = CARTESIAN_POINT ( 'NONE',  ( 0.1167790944451423257, 0.2124999999241334314, -0.2819296736111110424 ) ) ;
#15394 = ORIENTED_EDGE ( 'NONE', *, *, #22270, .F. ) ;
#15395 = CARTESIAN_POINT ( 'NONE',  ( 0.2819296736111110979, 4.338972222298087544, -3.452642723725051716E-17 ) ) ;
#15396 = CARTESIAN_POINT ( 'NONE',  ( -0.1236067977499789583, 0.1982142855192009223, -0.3804226065180614791 ) ) ;
#15397 = AXIS2_PLACEMENT_3D ( 'NONE', #3642, #14632, #23998 ) ;
#15398 = CARTESIAN_POINT ( 'NONE',  ( 0.2819296736111110424, 4.898000000075866112, -0.1167790944451423396 ) ) ;
#15399 = CARTESIAN_POINT ( 'NONE',  ( -0.1167790944451423119, 4.120222222298087544, -0.2819296736111110979 ) ) ;
#15400 = DIRECTION ( 'NONE',  ( 0.3266093577730910247, -0.7067687497613774905, 0.6275382552289447968 ) ) ;
#15401 = FACE_OUTER_BOUND ( 'NONE', #11457, .T. ) ;
#15402 = CARTESIAN_POINT ( 'NONE',  ( -1.910449006669871087E-17, 3.821611111262843252, -0.3119999999999999996 ) ) ;
#15403 =( BOUNDED_CURVE ( )  B_SPLINE_CURVE ( 2, ( #12953, #3780, #13068, #18772, #22068, #9509, #15008, #22429, #10989 ),
 .UNSPECIFIED., .F., .T. ) 
 B_SPLINE_CURVE_WITH_KNOTS ( ( 3, 2, 2, 2, 3 ),
 ( 0.5803571428571426827, 0.5848214285714283811, 0.5892857142857141906, 0.5937500000000000000, 0.5982142857142856984 ),
 .UNSPECIFIED. ) 
 CURVE ( )  GEOMETRIC_REPRESENTATION_ITEM ( )  RATIONAL_B_SPLINE_CURVE ( ( 1.000000000000003775, 0.9238795325112829637, 1.000000000000000000, 0.9238795325112867385, 1.000000000000000000, 0.9238795325112867385, 1.000000000000000000, 0.9238795325112867385, 1.000000000000000000 ) ) 
 REPRESENTATION_ITEM ( '' )  );
#15404 = APPROVAL_PERSON_ORGANIZATION ( #21006, #20442, #2244 ) ;
#15405 = CARTESIAN_POINT ( 'NONE',  ( 0.3119999999999998885, 0.1256944444444441089, 0.1292346314604058410 ) ) ;
#15406 = VERTEX_POINT ( 'NONE', #4557 ) ;
#15407 = APPROVAL_DATE_TIME ( #281, #14947 ) ;
#15408 = CIRCLE ( 'NONE', #18516, 0.3125000000000000000 ) ;
#15409 = EDGE_CURVE ( 'NONE', #5661, #20947, #10060, .T. ) ;
#15410 = DIRECTION ( 'NONE',  ( -0.000000000000000000, -1.000000000000000000, -0.000000000000000000 ) ) ;
#15411 = CARTESIAN_POINT ( 'NONE',  ( -0.4116234456863258617, 2.853030769935284372, -2.698516184653834582 ) ) ;
#15412 = VERTEX_POINT ( 'NONE', #8691 ) ;
#15413 = CARTESIAN_POINT ( 'NONE',  ( -0.2819296736111110979, 0.07708333325746669074, -3.452642723725051716E-17 ) ) ;
#15414 = ORIENTED_EDGE ( 'NONE', *, *, #22341, .T. ) ;
#15415 = CARTESIAN_POINT ( 'NONE',  ( 0.2839469674206308025, 4.255952816943617378, -0.1292989629763649229 ) ) ;
#15416 = CARTESIAN_POINT ( 'NONE',  ( 0.08208976641704460175, 0.4938713286266801505, 0.4000323696459243128 ) ) ;
#15417 = CARTESIAN_POINT ( 'NONE',  ( 0.1776117012215460422, 4.760747979974951249, -0.2606188829398497497 ) ) ;
#15418 = CARTESIAN_POINT ( 'NONE',  ( -0.1116596296178199582, 0.01517857133102903239, -0.3436530038418508792 ) ) ;
#15419 = CARTESIAN_POINT ( 'NONE',  ( 0.09457430736025282392, 5.187965616402109958, -0.2748785845271523032 ) ) ;
#15420 = ORIENTED_EDGE ( 'NONE', *, *, #23620, .F. ) ;
#15421 = CC_DESIGN_APPROVAL ( #12871, ( #19708 ) ) ;
#15422 = CARTESIAN_POINT ( 'NONE',  ( 0.2923287055106771337, 0.2901785713310289783, 0.2123892367102621359 ) ) ;
#15423 = CARTESIAN_POINT ( 'NONE',  ( -0.5116234456863466562, 4.118954363223904735, 3.002430311359389759 ) ) ;
#15424 = CARTESIAN_POINT ( 'NONE',  ( -1.910449006669871087E-17, 4.036888888888888083, -0.3119999999999999996 ) ) ;
#15425 = CARTESIAN_POINT ( 'NONE',  ( -0.1993543840281266910, 4.012583333409198261, -0.1993543840281266910 ) ) ;
#15426 = LINE ( 'NONE', #13610, #9863 ) ;
#15427 = CARTESIAN_POINT ( 'NONE',  ( -0.09460153516617859915, 5.193837599247971504, 0.2723203693900976829 ) ) ;
#15428 = AXIS2_PLACEMENT_3D ( 'NONE', #9646, #14898, #7813 ) ;
#15429 = CARTESIAN_POINT ( 'NONE',  ( -0.3119999999999999996, 4.554250000151733424, -0.1292346314604056468 ) ) ;
#15430 = CARTESIAN_POINT ( 'NONE',  ( -0.1993543840281266910, 4.915361111186976828, -0.1993543840281266910 ) ) ;
#15431 = EDGE_CURVE ( 'NONE', #13196, #23444, #12931, .T. ) ;
#15432 = ADVANCED_FACE ( 'NONE', ( #10899 ), #17945, .T. ) ;
#15433 = CARTESIAN_POINT ( 'NONE',  ( -0.1993543840281266910, 4.234805555631421470, -0.1993543840281266910 ) ) ;
#15434 = ORIENTED_EDGE ( 'NONE', *, *, #13694, .F. ) ;
#15435 = CARTESIAN_POINT ( 'NONE',  ( 0.1116596296178199860, 0.2937499999024575925, -0.3436530038418508792 ) ) ;
#15436 = ORIENTED_EDGE ( 'NONE', *, *, #995, .T. ) ;
#15437 = SECURITY_CLASSIFICATION ( '', '', #4867 ) ;
#15438 = ORIENTED_EDGE ( 'NONE', *, *, #5933, .F. ) ;
#15439 = PERSON_AND_ORGANIZATION ( #15518, #2538 ) ;
#15440 = EDGE_CURVE ( 'NONE', #9682, #2851, #3326, .T. ) ;
#15441 = DIRECTION ( 'NONE',  ( 0.7071067811865475727, 0.000000000000000000, 0.7071067811865475727 ) ) ;
#15442 = DIRECTION ( 'NONE',  ( -0.000000000000000000, -1.000000000000000000, -0.000000000000000000 ) ) ;
#15443 = CARTESIAN_POINT ( 'NONE',  ( 0.3119999999999999996, 0.01458333318160040526, -0.1292346314604056468 ) ) ;
#15444 = CIRCLE ( 'NONE', #6490, 0.2501339745962155581 ) ;
#15445 = CARTESIAN_POINT ( 'NONE',  ( 0.2928594795036059129, 4.415712943899434251, 0.1100155955557257648 ) ) ;
#15446 = CARTESIAN_POINT ( 'NONE',  ( -0.5116234456863258950, 4.559812086079793048, -2.640781157734871876 ) ) ;
#15447 = CARTESIAN_POINT ( 'NONE',  ( 0.000000000000000000, 3.700000000000000622, -0.4000000000000000222 ) ) ;
#15448 = CARTESIAN_POINT ( 'NONE',  ( 0.1954553509668046640, -0.1954553509668047195, 0.2758333333333367055 ) ) ;
#15449 = CARTESIAN_POINT ( 'NONE',  ( 0.1167790944451423535, 0.5388888888130223265, 0.2819296736111110979 ) ) ;
#15450 = CARTESIAN_POINT ( 'NONE',  ( -0.2764156081756484196, -0.1144950937579609362, 0.4320833333333378157 ) ) ;
#15451 = ORIENTED_EDGE ( 'NONE', *, *, #19771, .T. ) ;
#15452 = CARTESIAN_POINT ( 'NONE',  ( 0.2819296736111110979, 4.727861111186976828, -3.452642723725051716E-17 ) ) ;
#15453 = CARTESIAN_POINT ( 'NONE',  ( 0.000000000000000000, 0.000000000000000000, 1.326383476483184332 ) ) ;
#15454 = CARTESIAN_POINT ( 'NONE',  ( -0.2819296736111110424, 4.682722222298087544, -0.1167790944451423119 ) ) ;
#15455 = CARTESIAN_POINT ( 'NONE',  ( 0.4581189881604794123, -0.2644951211353317455, 0.3941886329748525153 ) ) ;
#15456 = CARTESIAN_POINT ( 'NONE',  ( 0.1864576510852719859, 4.871607367807203381, -0.2512479716031276178 ) ) ;
#15457 = CARTESIAN_POINT ( 'NONE',  ( 0.3394572874457115752, 3.700000000000000622, -0.09499999999999993172 ) ) ;
#15458 = CARTESIAN_POINT ( 'NONE',  ( 0.2728104005625097139, -0.05992465826480871532, 0.3905739001891366802 ) ) ;
#15459 = CARTESIAN_POINT ( 'NONE',  ( -0.2206173157302028232, 4.210499999999999687, -0.2206173157302028232 ) ) ;
#15460 = CARTESIAN_POINT ( 'NONE',  ( -0.1167790944451423119, 3.786888888964754063, -0.2819296736111110979 ) ) ;
#15461 = CARTESIAN_POINT ( 'NONE',  ( -0.4000000000000000222, 0.2249999999999999223, 0.1299678784931624920 ) ) ;
#15462 = ORIENTED_EDGE ( 'NONE', *, *, #10383, .F. ) ;
#15463 = VECTOR ( 'NONE', #18675, 39.37007874015748854 ) ;
#15464 = LINE ( 'NONE', #15108, #3882 ) ;
#15465 = EDGE_LOOP ( 'NONE', ( #755, #19296, #12995, #10413 ) ) ;
#15466 = CARTESIAN_POINT ( 'NONE',  ( 0.01239450642302288193, 4.710165812920179995, -0.3117901439589589874 ) ) ;
#15467 = CARTESIAN_POINT ( 'NONE',  ( 0.1906193665221117550, 4.133011534993895175, 0.2469985270587236048 ) ) ;
#15468 = CARTESIAN_POINT ( 'NONE',  ( -0.3155070326520292845, 1.931923388228935888E-17, -0.1009027777777772028 ) ) ;
#15469 = CARTESIAN_POINT ( 'NONE',  ( 4.282505654011733572E-07, 3.932722210548942776, -0.3119999999997061790 ) ) ;
#15470 = ORIENTED_EDGE ( 'NONE', *, *, #11530, .F. ) ;
#15471 = CARTESIAN_POINT ( 'NONE',  ( 0.3613381517857143232, -0.002678571526113826800, -0.1174058825155740587 ) ) ;
#15472 = AXIS2_PLACEMENT_3D ( 'NONE', #21550, #19243, #2547 ) ;
#15473 = CARTESIAN_POINT ( 'NONE',  ( 0.1167790944451423257, 0.4902777777019112215, -0.2819296736111110424 ) ) ;
#15474 = CARTESIAN_POINT ( 'NONE',  ( 0.000000000000000000, 0.1799999999999999933, -1.243000000000000105 ) ) ;
#15475 = LINE ( 'NONE', #7550, #4152 ) ;
#15476 = DIRECTION ( 'NONE',  ( -0.4999999999999995559, -0.8660254037844389297, 0.000000000000000000 ) ) ;
#15477 = CARTESIAN_POINT ( 'NONE',  ( -0.2764156081756484196, 0.1144950937579609918, 0.09180555555555744429 ) ) ;
#15478 = ORIENTED_EDGE ( 'NONE', *, *, #18257, .T. ) ;
#15479 = CARTESIAN_POINT ( 'NONE',  ( -0.3125685445540615781, 4.612853974748221120, -0.01387924731082778793 ) ) ;
#15480 = DIRECTION ( 'NONE',  ( 1.000000000000000000, 0.000000000000000000, 0.000000000000000000 ) ) ;
#15481 = CARTESIAN_POINT ( 'NONE',  ( 0.3119999999999999996, 4.745222222222221120, -3.820898013339742174E-17 ) ) ;
#15482 = CARTESIAN_POINT ( 'NONE',  ( -0.2206173157302027954, 0.2611111111111107386, -0.2206173157302028232 ) ) ;
#15483 = CARTESIAN_POINT ( 'NONE',  ( 0.3119999999999999996, 4.859805555555554157, -0.1292346314604056745 ) ) ;
#15484 = CARTESIAN_POINT ( 'NONE',  ( 5.178964085587577574E-17, 4.102861111186976828, 0.2819296736111110979 ) ) ;
#15485 = CARTESIAN_POINT ( 'NONE',  ( -5.428794840643969700E-10, 4.321611111277808170, -0.3119999999999999996 ) ) ;
#15486 = CARTESIAN_POINT ( 'NONE',  ( -0.3119999999999999996, 0.4798611109593782231, -0.1292346314604056745 ) ) ;
#15487 = CARTESIAN_POINT ( 'NONE',  ( 0.2669940301182540665, 4.812622197162082394, -0.1675650707301165887 ) ) ;
#15488 = ORIENTED_EDGE ( 'NONE', *, *, #8701, .T. ) ;
#15489 = CARTESIAN_POINT ( 'NONE',  ( -0.4805070082343984583, -0.2560807851245831546, 0.04413116910601652676 ) ) ;
#15490 = CARTESIAN_POINT ( 'NONE',  ( -0.2819296736111110979, 4.797305555631420582, 0.000000000000000000 ) ) ;
#15491 = CARTESIAN_POINT ( 'NONE',  ( -0.2233192592356400275, 0.3973214284738861291, 0.3073725909049499494 ) ) ;
#15492 = CARTESIAN_POINT ( 'NONE',  ( -0.1507708519810125880, 5.163359433834837198, 0.2585303382794060800 ) ) ;
#15493 = CIRCLE ( 'NONE', #20941, 0.01874999999999999237 ) ;
#15494 = EDGE_CURVE ( 'NONE', #23698, #12009, #19733, .T. ) ;
#15495 = CALENDAR_DATE ( 2026, 7, 10 ) ;
#15496 = CARTESIAN_POINT ( 'NONE',  ( -0.4795758971731803877, -0.04341642064210738533, 0.07439926260594938168 ) ) ;
#15497 = CARTESIAN_POINT ( 'NONE',  ( -0.4749999999999999778, 3.700000000000000622, 0.09499999999999995948 ) ) ;
#15498 = CARTESIAN_POINT ( 'NONE',  ( -0.2819296736111110979, 4.252166666742533074, -0.1167790944451422980 ) ) ;
#15499 = DATE_TIME_ROLE ( 'classification_date' ) ;
#15500 = CARTESIAN_POINT ( 'NONE',  ( 0.1292346314604031765, 4.311194444444443441, -0.3120000000000024420 ) ) ;
#15501 = CARTESIAN_POINT ( 'NONE',  ( 0.1144950937579611444, 0.2764156081756483641, -0.03319444444444354797 ) ) ;
#15502 = CARTESIAN_POINT ( 'NONE',  ( -0.3125000000000000000, 1.913510623667739771E-17, 0.3452777777777818469 ) ) ;
#15503 = CARTESIAN_POINT ( 'NONE',  ( -0.2819296736111110979, 0.4694444443685777957, 0.1167790944451422425 ) ) ;
#15504 = CARTESIAN_POINT ( 'NONE',  ( 1.998815303304994018, 2.291712385858714285, -2.661240473580833488 ) ) ;
#15505 = CARTESIAN_POINT ( 'NONE',  ( -0.4000000000000000222, 0.1499999999999999667, -4.898587196589413075E-17 ) ) ;
#15506 = CARTESIAN_POINT ( 'NONE',  ( 0.1236067977499789028, 0.3857142857142856207, 0.3804226065180614791 ) ) ;
#15507 = CARTESIAN_POINT ( 'NONE',  ( -0.2230971623002954152, -0.2230971623002953874, 0.1803472222222246291 ) ) ;
#15508 = FACE_OUTER_BOUND ( 'NONE', #17866, .T. ) ;
#15509 = CARTESIAN_POINT ( 'NONE',  ( -0.1294417382415922191, 0.3125000000000000000, 0.3834722222222263222 ) ) ;
#15510 = CARTESIAN_POINT ( 'NONE',  ( 0.1167790944451423119, 0.4347222221463555858, -0.2819296736111110979 ) ) ;
#15511 = CARTESIAN_POINT ( 'NONE',  ( 0.1167790944451423257, 0.2680555554796889561, -0.2819296736111110424 ) ) ;
#15512 = ORIENTED_EDGE ( 'NONE', *, *, #21873, .T. ) ;
#15513 = CARTESIAN_POINT ( 'NONE',  ( -0.2819296736111110424, 4.252166666742533074, -0.1167790944451423119 ) ) ;
#15514 = VECTOR ( 'NONE', #10718, 39.37007874015748143 ) ;
#15515 = CARTESIAN_POINT ( 'NONE',  ( 0.3236067977499789694, 0.2410714283763437660, 0.2351141009169893659 ) ) ;
#15516 = CARTESIAN_POINT ( 'NONE',  ( 0.1167790944451422702, 4.793833333409199149, -0.2819296736111110424 ) ) ;
#15517 = CARTESIAN_POINT ( 'NONE',  ( 1.652571746775178152, 2.291712385858714285, -2.061529041877830704 ) ) ;
#15518 = PERSON ( 'UNSPECIFIED', 'UNSPECIFIED', 'UNSPECIFIED', ('UNSPECIFIED'), ('UNSPECIFIED'), ('UNSPECIFIED') ) ;
#15519 = EDGE_LOOP ( 'NONE', ( #4996, #8839, #2513, #21847 ) ) ;
#15520 = DIRECTION ( 'NONE',  ( -1.000000000000000000, 0.000000000000000000, -0.000000000000000000 ) ) ;
#15521 = CARTESIAN_POINT ( 'NONE',  ( -0.1292346314604057023, 3.957027777929510215, 0.3119999999999998885 ) ) ;
#15522 = CARTESIAN_POINT ( 'NONE',  ( 0.3125000000000000000, 3.827021247335477694E-17, 1.326383476483184332 ) ) ;
#15523 =( NAMED_UNIT ( * ) PLANE_ANGLE_UNIT ( ) SI_UNIT ( $, .RADIAN. ) );
#15524 = ORIENTED_EDGE ( 'NONE', *, *, #5591, .F. ) ;
#15525 = CIRCLE ( 'NONE', #23296, 0.6396424860381280109 ) ;
#15526 = PERSON_AND_ORGANIZATION ( #15518, #2538 ) ;
#15527 = CARTESIAN_POINT ( 'NONE',  ( 0.1236067977499789028, 0.3142857142857142239, 0.3804226065180614791 ) ) ;
#15528 = CARTESIAN_POINT ( 'NONE',  ( -8.251178249108312710E-07, 5.016022433328296337, 0.3119999999976432181 ) ) ;
#15529 = VERTEX_POINT ( 'NONE', #10784 ) ;
#15530 = CARTESIAN_POINT ( 'NONE',  ( -5.178964085587577574E-17, 0.09097222214635558579, 0.2819296736111110979 ) ) ;
#15531 = CARTESIAN_POINT ( 'NONE',  ( -0.4000000000000000222, 0.007142857142857113144, -4.898587196589413075E-17 ) ) ;
#15532 = CARTESIAN_POINT ( 'NONE',  ( 0.2681267372835091090, 0.3756399061183655630, 0.4344383781808607847 ) ) ;
#15533 = CARTESIAN_POINT ( 'NONE',  ( 0.08432056328971544723, 4.096951260793152194, -0.3033353371696297374 ) ) ;
#15534 = CARTESIAN_POINT ( 'NONE',  ( 0.2233192592356399164, 0.1973214284738861179, 0.3073725909049500604 ) ) ;
#15535 = FACE_OUTER_BOUND ( 'NONE', #8027, .T. ) ;
#15536 = ORIENTED_EDGE ( 'NONE', *, *, #5846, .T. ) ;
#15537 = CARTESIAN_POINT ( 'NONE',  ( -0.1116596296178200276, 0.3473214284738860846, 0.3436530038418508792 ) ) ;
#15538 = CARTESIAN_POINT ( 'NONE',  ( -0.3119999999999999996, 4.047305555555555046, -0.1292346314604056468 ) ) ;
#15539 = EDGE_CURVE ( 'NONE', #10051, #9670, #16431, .T. ) ;
#15540 = CARTESIAN_POINT ( 'NONE',  ( 0.2819296736111110979, 3.988277777853643347, 0.1167790944451422425 ) ) ;
#15541 =( BOUNDED_CURVE ( )  B_SPLINE_CURVE ( 2, ( #23021, #13667, #15716, #20721, #19373, #21081, #4133, #15359, #7797, #22787, #8029, #5843, #356 ),
 .UNSPECIFIED., .F., .T. ) 
 B_SPLINE_CURVE_WITH_KNOTS ( ( 3, 2, 2, 2, 2, 2, 3 ),
 ( 0.2500000000000000000, 0.2571428571428571175, 0.2714285714285714080, 0.2857142857142856984, 0.2999999999999999889, 0.3142857142857142794, 0.3214285714285714524 ),
 .UNSPECIFIED. ) 
 CURVE ( )  GEOMETRIC_REPRESENTATION_ITEM ( )  RATIONAL_B_SPLINE_CURVE ( ( 0.9755282581475768211, 0.9755282581475768211, 1.000000000000000000, 0.9510565162951535312, 1.000000000000000000, 0.9510565162951535312, 1.000000000000000000, 0.9510565162951535312, 1.000000000000000000, 0.9510565162951535312, 1.000000000000000000, 0.9755282581475765991, 0.9755282581475767101 ) ) 
 REPRESENTATION_ITEM ( '' )  );
#15542 =( BOUNDED_CURVE ( )  B_SPLINE_CURVE ( 2, ( #8172, #21468, #4752, #17332, #626, #8057, #15505, #13691, #4398, #17450, #21939, #18048, #23757 ),
 .UNSPECIFIED., .F., .F. ) 
 B_SPLINE_CURVE_WITH_KNOTS ( ( 3, 2, 2, 2, 2, 2, 3 ),
 ( 0.4642857142857143016, 0.4714285714285714191, 0.4857142857142857095, 0.5000000000000000000, 0.5142857142857142350, 0.5285714285714285809, 0.5357142857142856984 ),
 .UNSPECIFIED. ) 
 CURVE ( )  GEOMETRIC_REPRESENTATION_ITEM ( )  RATIONAL_B_SPLINE_CURVE ( ( 0.9755282581475767101, 0.9755282581475768211, 1.000000000000000000, 0.9510565162951535312, 1.000000000000000000, 0.9510565162951535312, 1.000000000000000000, 0.9510565162951535312, 1.000000000000000000, 0.9510565162951535312, 1.000000000000000000, 0.9755282581475768211, 0.9755282581475768211 ) ) 
 REPRESENTATION_ITEM ( '' )  );
#15543 = CARTESIAN_POINT ( 'NONE',  ( 0.02891941893387090998, 5.043051531045750657, -0.3110769485290388325 ) ) ;
#15544 = CARTESIAN_POINT ( 'NONE',  ( -0.06631323151226614643, 5.164881977199022423, -0.2908543057123224029 ) ) ;
#15545 = VECTOR ( 'NONE', #14371, 39.37007874015748143 ) ;
#15546 = CARTESIAN_POINT ( 'NONE',  ( 0.3119999999999999996, 4.529944444596176290, -3.820898013339742174E-17 ) ) ;
#15547 = EDGE_CURVE ( 'NONE', #20545, #9930, #2924, .T. ) ;
#15548 = CARTESIAN_POINT ( 'NONE',  ( 5.178964085587577574E-17, 4.991750000075866112, 0.2819296736111110979 ) ) ;
#15549 = ORIENTED_EDGE ( 'NONE', *, *, #2915, .T. ) ;
#15550 = CARTESIAN_POINT ( 'NONE',  ( 0.1167790944451424368, 4.036888888964754507, 0.2819296736111110424 ) ) ;
#15551 = EDGE_LOOP ( 'NONE', ( #3218, #15414, #9315, #23641 ) ) ;
#15552 = ORIENTED_EDGE ( 'NONE', *, *, #19918, .T. ) ;
#15553 = APPLICATION_PROTOCOL_DEFINITION ( 'international standard', 'config_control_design', 1994, #20566 ) ;
#15554 = CARTESIAN_POINT ( 'NONE',  ( -0.3077469291169039889, -0.3525961953783998126, 0.4304954382810342595 ) ) ;
#15555 = LINE ( 'NONE', #8342, #8888 ) ;
#15556 = CARTESIAN_POINT ( 'NONE',  ( -0.2819296736111110979, 3.755638888964754951, 0.000000000000000000 ) ) ;
#15557 = AXIS2_PLACEMENT_3D ( 'NONE', #22770, #95, #19114 ) ;
#15558 = B_SPLINE_CURVE_WITH_KNOTS ( 'NONE', 3,
 ( #9317, #5414, #12999, #7486, #13119, #18701, #21996, #9072, #16520, #2000, #9437, #7604, #15055, #1755, #4830, #3342, #10798, #9198, #7133, #5295, #23937, #24059, #7368, #14818, #22236, #12782, #2914, #10488, #23501, #1662, #6817, #14727, #14259, #22142 ),
 .UNSPECIFIED., .F., .F.,
 ( 4, 2, 2, 2, 2, 2, 2, 2, 2, 2, 2, 2, 2, 2, 2, 2, 4 ),
 ( 0.02754951627422656119, 0.02882399678901069462, 0.03009847730379482805, 0.03137295781857896149, 0.03264743833336309492, 0.03392191884814722835, 0.03519639936293136179, 0.03647087987771549522, 0.03774536039249962865, 0.03901984090728376209, 0.04029432142206789552, 0.04156880193685202896, 0.04284328245163616239, 0.04411776296642029582, 0.04539224348120442926, 0.04666672399598856269, 0.04794120451077269612 ),
 .UNSPECIFIED. ) ;
#15559 = CARTESIAN_POINT ( 'NONE',  ( 0.1849291740725004518, 5.155468161834985352, -0.2375778761813798490 ) ) ;
#15560 = CARTESIAN_POINT ( 'NONE',  ( 0.1767089000523858477, 4.410255657018761433, 0.2583257397394467803 ) ) ;
#15561 = CARTESIAN_POINT ( 'NONE',  ( -0.4687500000000003886, 0.2598076211353315124, 0.3779506566538943790 ) ) ;
#15562 = CARTESIAN_POINT ( 'NONE',  ( 0.04810232026109438619, -0.5134939898138474179, 0.05816208736415689334 ) ) ;
#15563 = CARTESIAN_POINT ( 'NONE',  ( 0.1144950937579609085, -0.2764156081756484751, 0.1612500000000024469 ) ) ;
#15564 = DIRECTION ( 'NONE',  ( 0.000000000000000000, 0.000000000000000000, -1.000000000000000000 ) ) ;
#15565 = CARTESIAN_POINT ( 'NONE',  ( 0.2764156081756484196, -5.077672346800151106E-17, 0.4563888888888936735 ) ) ;
#15566 = ORIENTED_EDGE ( 'NONE', *, *, #3366, .F. ) ;
#15567 = CARTESIAN_POINT ( 'NONE',  ( 0.2819296736111110979, 4.835500000075866112, 0.1167790944451422425 ) ) ;
#15568 = DIRECTION ( 'NONE',  ( 0.000000000000000000, 1.000000000000000000, 0.000000000000000000 ) ) ;
#15569 = CARTESIAN_POINT ( 'NONE',  ( -0.2819296736111110424, 4.738277777853642903, -0.1167790944451423119 ) ) ;
#15570 = CARTESIAN_POINT ( 'NONE',  ( -0.01779695850694028303, 4.155454319339479063, -0.3115646979797883076 ) ) ;
#15571 = DIRECTION ( 'NONE',  ( -0.000000000000000000, -1.000000000000000000, -0.000000000000000000 ) ) ;
#15572 = CARTESIAN_POINT ( 'NONE',  ( 0.000000000000000000, 0.4997679491924311157, 0.000000000000000000 ) ) ;
#15573 = LINE ( 'NONE', #10456, #18997 ) ;
#15574 = CARTESIAN_POINT ( 'NONE',  ( 0.1292346314604058410, 4.290361111111110404, 0.3119999999999998885 ) ) ;
#15575 = CARTESIAN_POINT ( 'NONE',  ( 0.2206173157302027954, 5.092444444596176290, -0.2206173157302028232 ) ) ;
#15576 = EDGE_CURVE ( 'NONE', #9147, #23278, #4614, .T. ) ;
#15577 = CARTESIAN_POINT ( 'NONE',  ( -5.731347020009612645E-17, 0.5527777776260448528, 0.3119999999999999996 ) ) ;
#15578 = AXIS2_PLACEMENT_3D ( 'NONE', #16220, #21462, #14146 ) ;
#15579 = ORIENTED_EDGE ( 'NONE', *, *, #8853, .T. ) ;
#15580 = CARTESIAN_POINT ( 'NONE',  ( 0.2209708691207961651, 0.2209708691207959985, 0.2063888888888915363 ) ) ;
#15581 = VERTEX_POINT ( 'NONE', #15717 ) ;
#15582 = CARTESIAN_POINT ( 'NONE',  ( 0.0002156662915977773556, 4.710494205284167180, -0.3119999301816606674 ) ) ;
#15583 = UNCERTAINTY_MEASURE_WITH_UNIT (LENGTH_MEASURE( 1.000000000000000082E-05 ), #5744, 'distance_accuracy_value', 'NONE');
#15584 = CARTESIAN_POINT ( 'NONE',  ( 0.2704457082507048526, 4.136385615343296074, 0.1578283642472184667 ) ) ;
#15585 = CARTESIAN_POINT ( 'NONE',  ( -0.3155070326520293400, 0.1306872919485614903, 0.006736111111112530123 ) ) ;
#15586 = CARTESIAN_POINT ( 'NONE',  ( 3.061616997868383018E-17, 5.954200000000001936, 0.2500000000000000000 ) ) ;
#15587 = AXIS2_PLACEMENT_3D ( 'NONE', #17630, #23337, #21524 ) ;
#15588 = CARTESIAN_POINT ( 'NONE',  ( 2.326421213736078119E-17, 0.01160714275960046671, -0.3799334167787516425 ) ) ;
#15589 = AXIS2_PLACEMENT_3D ( 'NONE', #19484, #2666, #2778 ) ;
#15590 = EDGE_CURVE ( 'NONE', #23326, #1317, #22231, .T. ) ;
#15591 = CARTESIAN_POINT ( 'NONE',  ( -0.1993543840281267465, 0.4034722221463555858, 0.1993543840281266633 ) ) ;
#15592 = CARTESIAN_POINT ( 'NONE',  ( -0.01963737563095444699, 5.206640035683668621, 0.2814148482456156897 ) ) ;
#15593 = CARTESIAN_POINT ( 'NONE',  ( 0.7108475124358387687, 1.999640111863030700, -2.834606755790658461 ) ) ;
#15594 = CARTESIAN_POINT ( 'NONE',  ( 0.003366903179264894679, 0.5383683782340862312, 0.05892738626661216117 ) ) ;
#15595 = CARTESIAN_POINT ( 'NONE',  ( -0.1954553509668046918, -0.1954553509668046640, 0.1577777777777801815 ) ) ;
#15596 = VERTEX_POINT ( 'NONE', #19021 ) ;
#15597 = DIRECTION ( 'NONE',  ( 1.000000000000000000, 0.000000000000000000, 0.000000000000000000 ) ) ;
#15598 = FACE_OUTER_BOUND ( 'NONE', #16406, .T. ) ;
#15599 = PLANE ( 'NONE',  #8663 ) ;
#15600 = CARTESIAN_POINT ( 'NONE',  ( 0.1292346314604056745, 0.1395833333333330317, -0.3119999999999999996 ) ) ;
#15601 = CARTESIAN_POINT ( 'NONE',  ( -0.2206173157302028232, 5.043833333333332725, -0.2206173157302028232 ) ) ;
#15602 = B_SPLINE_CURVE_WITH_KNOTS ( 'NONE', 3,
 ( #4351, #23000, #6303, #18879 ),
 .UNSPECIFIED., .F., .F.,
 ( 4, 4 ),
 ( 1.008999589182314829E-06, 0.001469413801632195879 ),
 .UNSPECIFIED. ) ;
#15603 = CARTESIAN_POINT ( 'NONE',  ( 0.2819296736111110979, 3.891055555631421914, 0.1167790944451422425 ) ) ;
#15604 = ADVANCED_FACE ( 'NONE', ( #6444 ), #22907, .T. ) ;
#15605 = CARTESIAN_POINT ( 'NONE',  ( -0.2977100099089716734, 3.659999999999999698, -0.09499999999999995948 ) ) ;
#15606 = CARTESIAN_POINT ( 'NONE',  ( -0.3309966345752030081, 0.3501648812924316179, 0.4216785431538761508 ) ) ;
#15607 = FACE_OUTER_BOUND ( 'NONE', #14085, .T. ) ;
#15608 = ORIENTED_EDGE ( 'NONE', *, *, #17515, .F. ) ;
#15609 = ORIENTED_EDGE ( 'NONE', *, *, #11555, .T. ) ;
#15610 = CARTESIAN_POINT ( 'NONE',  ( -0.08166533652539130494, 3.990609059424373051, -0.3038794758048473654 ) ) ;
#15611 = CARTESIAN_POINT ( 'NONE',  ( 0.2819296736111110979, 4.654944444520309865, 0.1167790944451422425 ) ) ;
#15612 = CARTESIAN_POINT ( 'NONE',  ( 0.08494034609768591482, 0.4922255456806988727, 0.06591861138178030377 ) ) ;
#15613 = VECTOR ( 'NONE', #10499, 39.37007874015748143 ) ;
#15614 = CARTESIAN_POINT ( 'NONE',  ( -0.5116234456863258950, 4.559812086079793048, -2.813986238491759551 ) ) ;
#15615 = VECTOR ( 'NONE', #1489, 39.37007874015748854 ) ;
#15616 = APPLICATION_PROTOCOL_DEFINITION ( 'international standard', 'config_control_design', 1994, #23042 ) ;
#15617 = CARTESIAN_POINT ( 'NONE',  ( -0.4805070082343984583, -0.2560807851245831546, 0.04413116910601656145 ) ) ;
#15618 = FACE_OUTER_BOUND ( 'NONE', #7916, .T. ) ;
#15619 = DIRECTION ( 'NONE',  ( 1.000000000000000000, 0.000000000000000000, -6.148297094540788948E-16 ) ) ;
#15620 = CARTESIAN_POINT ( 'NONE',  ( -0.1167790944451423119, 4.245222222298088433, -0.2819296736111110979 ) ) ;
#15621 = CARTESIAN_POINT ( 'NONE',  ( -0.01840724122558156858, 4.044333937968741743, -0.3114566890697244017 ) ) ;
#15622 = CARTESIAN_POINT ( 'NONE',  ( -0.2764156081756484196, 0.1144950937579609918, -0.01930555555555454883 ) ) ;
#15623 = CARTESIAN_POINT ( 'NONE',  ( -0.1060554323913378977, 4.559812086079793048, -2.874935959385435336 ) ) ;
#15624 = CARTESIAN_POINT ( 'NONE',  ( 0.1993543840281266355, 0.4868055554796889006, 0.1993543840281267465 ) ) ;
#15625 = CARTESIAN_POINT ( 'NONE',  ( -0.3119999999999999996, 0.4347222222222218435, -3.820898013339742174E-17 ) ) ;
#15626 = LINE ( 'NONE', #8293, #20655 ) ;
#15627 = CARTESIAN_POINT ( 'NONE',  ( -0.4000000000000000222, 0.3642857142857142128, -4.898587196589413075E-17 ) ) ;
#15628 = CARTESIAN_POINT ( 'NONE',  ( 0.3155070326520292845, -5.795770164686806123E-17, 0.2567361111111141070 ) ) ;
#15629 = PLANE ( 'NONE',  #23494 ) ;
#15630 = CARTESIAN_POINT ( 'NONE',  ( 0.3124999999999999445, 0.1294417382415923023, 0.3695833333333372606 ) ) ;
#15631 = CARTESIAN_POINT ( 'NONE',  ( -0.2819296736111111534, 0.5111111110352445364, 0.1167790944451422563 ) ) ;
#15632 = CARTESIAN_POINT ( 'NONE',  ( -0.2819296736111110979, 0.2854166665908000611, -3.452642723725051716E-17 ) ) ;
#15633 = VECTOR ( 'NONE', #289, 39.37007874015748854 ) ;
#15634 = CARTESIAN_POINT ( 'NONE',  ( -0.2819296736111110424, 4.148000000075866112, 0.1167790944451424923 ) ) ;
#15635 = CARTESIAN_POINT ( 'NONE',  ( -0.1236067977499790416, 0.2267857140906295033, 0.3804226065180614236 ) ) ;
#15636 = CARTESIAN_POINT ( 'NONE',  ( 5.178964085587577574E-17, 4.547305555631421470, 0.2819296736111110979 ) ) ;
#15637 = EDGE_CURVE ( 'NONE', #15596, #12509, #17617, .T. ) ;
#15638 = CARTESIAN_POINT ( 'NONE',  ( 0.000000000000000000, 5.579732050807569621, -0.2510000000000000009 ) ) ;
#15639 = EDGE_LOOP ( 'NONE', ( #11525, #17463, #579, #18458 ) ) ;
#15640 = ORIENTED_EDGE ( 'NONE', *, *, #21645, .F. ) ;
#15641 = CARTESIAN_POINT ( 'NONE',  ( -0.08492194567810140704, 0.4922361691679148499, 0.06591465713331619292 ) ) ;
#15642 = CARTESIAN_POINT ( 'NONE',  ( -0.3119999999999998885, 3.894527777929509771, 0.1292346314604058410 ) ) ;
#15643 = LINE ( 'NONE', #15763, #15762 ) ;
#15644 = ORIENTED_EDGE ( 'NONE', *, *, #6637, .F. ) ;
#15645 = PERSON_AND_ORGANIZATION ( #15518, #2538 ) ;
#15646 = CARTESIAN_POINT ( 'NONE',  ( 0.3236067977499789694, 0.4553571426620579565, 0.2351141009169893659 ) ) ;
#15647 = CARTESIAN_POINT ( 'NONE',  ( -0.3032932187877268593, 5.000078586144176995, -0.07417139457035222538 ) ) ;
#15648 = EDGE_LOOP ( 'NONE', ( #16481, #2374, #18339, #8801 ) ) ;
#15649 = CARTESIAN_POINT ( 'NONE',  ( -0.2819296736111110979, 0.02152777770191114173, -3.452642723725051716E-17 ) ) ;
#15650 = ORIENTED_EDGE ( 'NONE', *, *, #2331, .T. ) ;
#15651 = CARTESIAN_POINT ( 'NONE',  ( 0.08155431767186305247, 4.240654305037732996, 0.3039018303971695034 ) ) ;
#15652 = DIRECTION ( 'NONE',  ( -8.881784197001252323E-16, 0.000000000000000000, 1.000000000000000000 ) ) ;
#15653 = CARTESIAN_POINT ( 'NONE',  ( 0.1735223483235301123, 4.076898470827504894, 0.2600906113308195655 ) ) ;
#15654 = CARTESIAN_POINT ( 'NONE',  ( -0.2923287055106771337, 0.2366071427596004584, -0.2123892367102620804 ) ) ;
#15655 = CARTESIAN_POINT ( 'NONE',  ( 0.2010820074625671305, 5.184841366458968537, -0.2109359274478957158 ) ) ;
#15656 = APPROVAL ( #8598, 'UNSPECIFIED' ) ;
#15657 = DIRECTION ( 'NONE',  ( -0.000000000000000000, -1.000000000000000000, -0.000000000000000000 ) ) ;
#15658 = CARTESIAN_POINT ( 'NONE',  ( 1.846908021952178069, 1.442300479962384641, -4.378300479962384806 ) ) ;
#15659 = CARTESIAN_POINT ( 'NONE',  ( 0.2819296736111110424, 3.995222222298087544, -0.1167790944451423396 ) ) ;
#15660 = CARTESIAN_POINT ( 'NONE',  ( 1.990666666666680795, -0.9453333333333302502, -0.9953333333333292954 ) ) ;
#15661 = CARTESIAN_POINT ( 'NONE',  ( -0.2841123412848098884, 5.182397235849433237, 0.07086212028873112301 ) ) ;
#15662 = FACE_OUTER_BOUND ( 'NONE', #5652, .T. ) ;
#15663 = CARTESIAN_POINT ( 'NONE',  ( 0.2206173157302027954, 4.481333333485065573, -0.2206173157302028232 ) ) ;
#15664 = CARTESIAN_POINT ( 'NONE',  ( 0.2819296736111110979, 4.898000000075865223, -0.1167790944451423396 ) ) ;
#15665 = ORIENTED_EDGE ( 'NONE', *, *, #18696, .F. ) ;
#15666 = EDGE_CURVE ( 'NONE', #20523, #4205, #9473, .T. ) ;
#15667 = CARTESIAN_POINT ( 'NONE',  ( 0.2819296736111110979, 3.988277777853643347, 0.1167790944451422425 ) ) ;
#15668 = ORIENTED_EDGE ( 'NONE', *, *, #19742, .T. ) ;
#15669 = AXIS2_PLACEMENT_3D ( 'NONE', #6299, #10096, #812 ) ;
#15670 = ORIENTED_EDGE ( 'NONE', *, *, #4570, .F. ) ;
#15671 = ORIENTED_EDGE ( 'NONE', *, *, #7509, .T. ) ;
#15672 = APPROVAL_STATUS ( 'not_yet_approved' ) ;
#15673 = ORIENTED_EDGE ( 'NONE', *, *, #5401, .T. ) ;
#15674 = CARTESIAN_POINT ( 'NONE',  ( -0.07572755880264375739, -0.4860218594902851463, 0.4166771511014251694 ) ) ;
#15675 = CARTESIAN_POINT ( 'NONE',  ( -0.3125000000000010547, 0.1294417382415911921, 0.2793055555555588598 ) ) ;
#15676 = CARTESIAN_POINT ( 'NONE',  ( 0.1292346314604057023, 0.05624999984826706961, 0.3119999999999998885 ) ) ;
#15677 = CARTESIAN_POINT ( 'NONE',  ( 0.01998333260083862140, 5.130840972916198339, 0.3061013181601511257 ) ) ;
#15678 = PRODUCT_DEFINITION ( 'UNKNOWN', '', #8009, #2422 ) ;
#15679 = CARTESIAN_POINT ( 'NONE',  ( -0.4584472689070020479, 0.2219065841078094181, 0.4063187442602073651 ) ) ;
#15680 = CARTESIAN_POINT ( 'NONE',  ( 0.3124999999999989453, -0.1294417382415934403, -0.07486111111111042049 ) ) ;
#15681 =( BOUNDED_CURVE ( )  B_SPLINE_CURVE ( 2, ( #10710, #3383, #15829, #3028, #10475, #23727, #17905, #18021, #14488 ),
 .UNSPECIFIED., .F., .T. ) 
 B_SPLINE_CURVE_WITH_KNOTS ( ( 3, 2, 2, 2, 3 ),
 ( 0.9017857142857141906, 0.9062499999999998890, 0.9107142857142855874, 0.9151785714285713969, 0.9196428571428570953 ),
 .UNSPECIFIED. ) 
 CURVE ( )  GEOMETRIC_REPRESENTATION_ITEM ( )  RATIONAL_B_SPLINE_CURVE ( ( 1.000000000000001998, 0.9238795325112848511, 1.000000000000000000, 0.9238795325112867385, 1.000000000000000000, 0.9238795325112867385, 1.000000000000000000, 0.9238795325112867385, 1.000000000000000000 ) ) 
 REPRESENTATION_ITEM ( '' )  );
#15682 =( BOUNDED_CURVE ( )  B_SPLINE_CURVE ( 1, ( #10127, #15724 ),
 .UNSPECIFIED., .F., .T. ) 
 B_SPLINE_CURVE_WITH_KNOTS ( ( 2, 2 ),
 ( 0.000000000000000000, 1.000000000000000000 ),
 .UNSPECIFIED. ) 
 CURVE ( )  GEOMETRIC_REPRESENTATION_ITEM ( )  RATIONAL_B_SPLINE_CURVE ( ( 0.9836823002065551158, 0.9836823002065551158 ) ) 
 REPRESENTATION_ITEM ( '' )  );
#15683 = CYLINDRICAL_SURFACE ( 'NONE', #14172, 0.3125000000000000000 ) ;
#15684 = CARTESIAN_POINT ( 'NONE',  ( 0.1144950937579609085, -0.2764156081756484751, 0.3834722222222265997 ) ) ;
#15685 = FACE_OUTER_BOUND ( 'NONE', #23335, .T. ) ;
#15686 = CARTESIAN_POINT ( 'NONE',  ( 0.2764156081756484196, -5.077672346800151106E-17, 0.1716666666666692431 ) ) ;
#15687 = ORIENTED_EDGE ( 'NONE', *, *, #5537, .T. ) ;
#15688 = CARTESIAN_POINT ( 'NONE',  ( 0.7108475124358382136, 4.111524471938507119, -3.019372695974962717 ) ) ;
#15689 = AXIS2_PLACEMENT_3D ( 'NONE', #21297, #6416, #13870 ) ;
#15690 = CARTESIAN_POINT ( 'NONE',  ( -0.1167790944451423257, 4.675777777853642903, -0.2819296736111110424 ) ) ;
#15691 = CARTESIAN_POINT ( 'NONE',  ( -0.3125000000000000000, 1.913510623667739771E-17, 0.3383333333333369830 ) ) ;
#15692 = CARTESIAN_POINT ( 'NONE',  ( -0.2989142788957511176, 0.3766842777223494143, -1.152193287665570942 ) ) ;
#15693 = CARTESIAN_POINT ( 'NONE',  ( 9.184850993605150903E-17, 0.000000000000000000, -0.7500000000000001110 ) ) ;
#15694 = CARTESIAN_POINT ( 'NONE',  ( 8.768852782367848672E-17, -0.5412658773652745392, 0.4425000000000000044 ) ) ;
#15695 = CARTESIAN_POINT ( 'NONE',  ( 0.1292346314604058410, 4.345916666666665762, 0.3119999999999998885 ) ) ;
#15696 = CARTESIAN_POINT ( 'NONE',  ( 0.2206173157302028787, 5.078555555707287006, 0.2206173157302027954 ) ) ;
#15697 = CARTESIAN_POINT ( 'NONE',  ( 0.3095665875726216210, 4.973302152571846158, 0.03932295407607730442 ) ) ;
#15698 = VERTEX_POINT ( 'NONE', #11830 ) ;
#15699 = DIMENSIONAL_EXPONENTS ( 1.000000000000000000, 0.000000000000000000, 0.000000000000000000, 0.000000000000000000, 0.000000000000000000, 0.000000000000000000, 0.000000000000000000 ) ;
#15700 = CARTESIAN_POINT ( 'NONE',  ( 4.589747744727345336E-07, 4.571629220806286753, 0.3119999999992840722 ) ) ;
#15701 = EDGE_LOOP ( 'NONE', ( #638, #23064, #17674, #4247 ) ) ;
#15702 = CARTESIAN_POINT ( 'NONE',  ( 0.2841390510945954739, 4.700384098082350803, -0.1288870310084711535 ) ) ;
#15703 = AXIS2_PLACEMENT_3D ( 'NONE', #8343, #21286, #15909 ) ;
#15704 = CARTESIAN_POINT ( 'NONE',  ( 0.03111664948054426727, 4.128053875489018587, 0.3119999999605160279 ) ) ;
#15705 = CARTESIAN_POINT ( 'NONE',  ( 0.000000000000000000, 0.3155070326520292845, -0.003680555555554220534 ) ) ;
#15706 = CARTESIAN_POINT ( 'NONE',  ( -0.08367912913462059732, -0.4929537096338480473, 0.07813342133392800481 ) ) ;
#15707 = ADVANCED_FACE ( 'NONE', ( #19249, #22339 ), #15599, .T. ) ;
#15708 = CARTESIAN_POINT ( 'NONE',  ( 0.2233192592356399997, 0.004464285616743319737, -0.3073725909049500049 ) ) ;
#15709 = CARTESIAN_POINT ( 'NONE',  ( 0.1167790944451423119, 0.1152777777019111383, -0.2819296736111110979 ) ) ;
#15710 = CARTESIAN_POINT ( 'NONE',  ( 0.1144950937579609085, -0.2764156081756484751, 0.1126388888888909395 ) ) ;
#15711 = CARTESIAN_POINT ( 'NONE',  ( -0.1294417382415922746, -0.3125000000000000000, 0.4112500000000045008 ) ) ;
#15712 = CARTESIAN_POINT ( 'NONE',  ( -0.1537937564252621903, -0.2409193255903078756, -0.07485594907830336875 ) ) ;
#15713 = CARTESIAN_POINT ( 'NONE',  ( 0.1144950937579611444, 0.2764156081756483641, 0.3001388888888924522 ) ) ;
#15714 = VERTEX_POINT ( 'NONE', #5642 ) ;
#15715 = CARTESIAN_POINT ( 'NONE',  ( -0.2905554862335017474, 4.616567866447413238, 0.1152557973630595062 ) ) ;
#15716 = CARTESIAN_POINT ( 'NONE',  ( 0.1236067977499789028, 0.09107142837634375765, 0.3804226065180614791 ) ) ;
#15717 = CARTESIAN_POINT ( 'NONE',  ( 0.4805070082343983473, 0.2560807851245830991, 0.04413116910601658921 ) ) ;
#15718 = CARTESIAN_POINT ( 'NONE',  ( -0.3119999999999999996, 0.4312499999999996336, -0.1292346314604056745 ) ) ;
#15719 = CARTESIAN_POINT ( 'NONE',  ( -0.3119999999999998885, 5.054249999999998799, 0.1292346314604058410 ) ) ;
#15720 = B_SPLINE_CURVE_WITH_KNOTS ( 'NONE', 3,
 ( #16812, #93, #11204, #1925, #9490, #22407, #5708, #2051, #219, #20584, #11325, #7657, #18755, #15107, #14872, #22288, #11039, #3587, #12888, #20419, #16526, #16409, #3714, #18469, #23944, #47, #21883, #7493, #11163, #22242, #20182, #19940, #1883, #23695, #23817, #16764, #7375, #8835, #7260, #20302, #20060, #9324, #16284, #9205, #12642, #5174 ),
 .UNSPECIFIED., .F., .F.,
 ( 4, 2, 2, 2, 2, 1, 2, 2, 1, 1, 1, 1, 2, 2, 2, 2, 2, 2, 1, 1, 2, 2, 1, 2, 2, 2, 4 ),
 ( 0.9753616152418370655, 0.9766508353774531193, 0.9779400555130691730, 0.9792292756486852268, 0.9795515806825892957, 0.9797127331995412192, 0.9797177692156959772, 0.9797228052318507352, 0.9797328772641602512, 0.9797530213287792833, 0.9797933094580172364, 0.9798738857164932536, 0.9805184957843013915, 0.9830969360555337211, 0.9856753763267659396, 0.9882538165979982692, 0.9908322568692305987, 0.9914768669370387366, 0.9917991719709426945, 0.9918797482294187118, 0.9919200363586567759, 0.9919401804232758080, 0.9919603244878947290, 0.9921214770048467635, 0.9934106971404627062, 0.9946999172760787600, 0.9959891374116947027 ),
 .UNSPECIFIED. ) ;
#15721 = CIRCLE ( 'NONE', #13028, 0.3150000000000000022 ) ;
#15722 = CARTESIAN_POINT ( 'NONE',  ( 0.1167790944451422702, 4.071611111186977716, -0.2819296736111110424 ) ) ;
#15723 = SPHERICAL_SURFACE ( 'NONE', #5349, 0.01874999999999999931 ) ;
#15724 = CARTESIAN_POINT ( 'NONE',  ( 0.1988756632394131918, 3.704359868413474199, -0.2404006459456452249 ) ) ;
#15725 = CYLINDRICAL_SURFACE ( 'NONE', #14155, 0.01874999999999997155 ) ;
#15726 = ORIENTED_EDGE ( 'NONE', *, *, #670, .F. ) ;
#15727 = ORIENTED_EDGE ( 'NONE', *, *, #23851, .F. ) ;
#15728 = CARTESIAN_POINT ( 'NONE',  ( -0.08166537602659873496, 4.013806181748617696, 0.3038794651914065725 ) ) ;
#15729 = CARTESIAN_POINT ( 'NONE',  ( -0.1993543840281266355, 4.637583333409198261, 0.1993543840281267465 ) ) ;
#15730 = CARTESIAN_POINT ( 'NONE',  ( 0.1116596296178199027, 0.3366071427596004084, 0.3436530038418508792 ) ) ;
#15731 = CARTESIAN_POINT ( 'NONE',  ( -0.2206173157302027676, 4.113277777777777366, 0.2206173157302028787 ) ) ;
#15732 = EDGE_CURVE ( 'NONE', #11161, #1661, #14127, .T. ) ;
#15733 = ADVANCED_FACE ( 'NONE', ( #17907 ), #4762, .F. ) ;
#15734 = APPROVAL_ROLE ( '' ) ;
#15735 = CARTESIAN_POINT ( 'NONE',  ( -0.4687500000000003886, 0.08781630462512594881, 0.08855667131757492816 ) ) ;
#15736 = CARTESIAN_POINT ( 'NONE',  ( 0.1144950937579611444, 0.2764156081756483641, 0.1265277777777799595 ) ) ;
#15737 = CARTESIAN_POINT ( 'NONE',  ( 0.2819296736111110979, 4.338972222298087544, -3.452642723725051716E-17 ) ) ;
#15738 = CALENDAR_DATE ( 2026, 7, 10 ) ;
#15739 = AXIS2_PLACEMENT_3D ( 'NONE', #8935, #23792, #23552 ) ;
#15740 = DIRECTION ( 'NONE',  ( -1.000000000000000000, 0.000000000000000000, 0.000000000000000000 ) ) ;
#15741 = EDGE_CURVE ( 'NONE', #8540, #6009, #22680, .T. ) ;
#15742 = CARTESIAN_POINT ( 'NONE',  ( -1.910449006669871087E-17, 4.870222222222222008, -0.3119999999999999996 ) ) ;
#15743 = CARTESIAN_POINT ( 'NONE',  ( -0.1144950937579609918, -0.2764156081756484196, 0.2168055555555584990 ) ) ;
#15744 = CARTESIAN_POINT ( 'NONE',  ( 0.2472135954999579166, 0.2464285714285713580, 0.3402603233408160732 ) ) ;
#15745 = CARTESIAN_POINT ( 'NONE',  ( -0.1167790944451424368, 0.07361111103524446697, 0.2819296736111110424 ) ) ;
#15746 = CARTESIAN_POINT ( 'NONE',  ( 1.910449006669871087E-17, 0.08749999999999966138, -0.3119999999999999996 ) ) ;
#15747 = CARTESIAN_POINT ( 'NONE',  ( -0.4223122635727385998, 0.2974437783094735499, 0.07051021533369884742 ) ) ;
#15748 = CARTESIAN_POINT ( 'NONE',  ( 0.3999999999999999667, 0.3249999999999997891, 0.1299678784931626307 ) ) ;
#15749 = CARTESIAN_POINT ( 'NONE',  ( -0.2230971623002953874, 0.2230971623002954152, 0.4442361111111156058 ) ) ;
#15750 = DIRECTION ( 'NONE',  ( 0.000000000000000000, 0.000000000000000000, -1.000000000000000000 ) ) ;
#15751 = FACE_OUTER_BOUND ( 'NONE', #13596, .T. ) ;
#15752 = CARTESIAN_POINT ( 'NONE',  ( -0.2819296736111110979, 0.5076388888130222155, -3.452642723725051716E-17 ) ) ;
#15753 = CARTESIAN_POINT ( 'NONE',  ( 0.1993543840281266910, 0.5423611110352445364, -0.1993543840281266910 ) ) ;
#15754 = CARTESIAN_POINT ( 'NONE',  ( -0.1167790944451423535, 4.154944444520309865, 0.2819296736111110424 ) ) ;
#15755 = CARTESIAN_POINT ( 'NONE',  ( 0.3999999999999999667, 0.3874999998049151739, 0.1299678784931626307 ) ) ;
#15756 = CARTESIAN_POINT ( 'NONE',  ( 0.1993543840281266633, 4.568138888964755395, -0.1993543840281266910 ) ) ;
#15757 = DIRECTION ( 'NONE',  ( -0.000000000000000000, -0.9961946980917454342, 0.08715574274765830465 ) ) ;
#15758 = EDGE_CURVE ( 'NONE', #23209, #12951, #4966, .T. ) ;
#15759 = CARTESIAN_POINT ( 'NONE',  ( 0.2840431067139673749, 5.082267742700584456, -0.1295341344031159247 ) ) ;
#15760 = CARTESIAN_POINT ( 'NONE',  ( 5.731347020009612645E-17, 4.786888888888888083, 0.3119999999999999996 ) ) ;
#15761 = CARTESIAN_POINT ( 'NONE',  ( -0.1292346314604057023, 3.790361111262843252, 0.3119999999999998885 ) ) ;
#15762 = VECTOR ( 'NONE', #23060, 39.37007874015748854 ) ;
#15763 = CARTESIAN_POINT ( 'NONE',  ( 1.222470958122163998, 2.291712385858714729, -0.8172771125692949168 ) ) ;
#15764 = ORIENTED_EDGE ( 'NONE', *, *, #1721, .T. ) ;
#15765 =( GEOMETRIC_REPRESENTATION_CONTEXT ( 3 ) GLOBAL_UNCERTAINTY_ASSIGNED_CONTEXT ( ( #13882 ) ) GLOBAL_UNIT_ASSIGNED_CONTEXT ( ( #12842, #2214, #3914 ) ) REPRESENTATION_CONTEXT ( 'NONE', 'WORKASPACE' ) );
#15766 = DATE_TIME_ROLE ( 'classification_date' ) ;
#15767 = ORIENTED_EDGE ( 'NONE', *, *, #10756, .F. ) ;
#15768 = CARTESIAN_POINT ( 'NONE',  ( -0.2324876215537165225, 5.107993264127207667, -0.2053580284920872856 ) ) ;
#15769 = CARTESIAN_POINT ( 'NONE',  ( -0.3133021733797068942, 4.558532991712811011, 0.02780185521819914310 ) ) ;
#15770 = CARTESIAN_POINT ( 'NONE',  ( 0.3119999999999999996, 0.6222222220704892726, 0.000000000000000000 ) ) ;
#15771 = VERTEX_POINT ( 'NONE', #950 ) ;
#15772 = CARTESIAN_POINT ( 'NONE',  ( 0.3120349077283414152, 4.253276283983363548, -0.04063966104624280873 ) ) ;
#15773 = CARTESIAN_POINT ( 'NONE',  ( -0.07676069278406914831, 4.736058685955594427, 0.3046265517824304214 ) ) ;
#15774 = CARTESIAN_POINT ( 'NONE',  ( 0.3105152002621879292, 4.084448063609871227, 0.03699839793702524443 ) ) ;
#15775 = VECTOR ( 'NONE', #21865, 39.37007874015748854 ) ;
#15776 = CARTESIAN_POINT ( 'NONE',  ( 0.2233192592356399997, 0.2901785713310290338, -0.3073725909049500049 ) ) ;
#15777 = CARTESIAN_POINT ( 'NONE',  ( 0.2786832587059077659, 5.181255304933189088, -0.09125116685248849113 ) ) ;
#15778 = CARTESIAN_POINT ( 'NONE',  ( 1.845714884748260509, 0.000000000000000000, -2.498788568296995916 ) ) ;
#15779 = DIRECTION ( 'NONE',  ( -0.7071067811865435759, 8.659560562354884787E-17, 0.7071067811865514585 ) ) ;
#15780 = CARTESIAN_POINT ( 'NONE',  ( -0.1993543840281266355, 3.748694444520309865, 0.1993543840281267465 ) ) ;
#15781 = CARTESIAN_POINT ( 'NONE',  ( 1.910449006669871087E-17, 0.08055555540382261515, -0.3119999999999999996 ) ) ;
#15782 = APPROVAL_PERSON_ORGANIZATION ( #14261, #8045, #7068 ) ;
#15783 = CARTESIAN_POINT ( 'NONE',  ( -0.03821718199043266234, 5.196224427665105061, 0.2847346366168296283 ) ) ;
#15784 = CARTESIAN_POINT ( 'NONE',  ( -0.2472135954999579444, 0.2017857140906293978, -0.3402603233408160732 ) ) ;
#15785 = CARTESIAN_POINT ( 'NONE',  ( -0.2206173157302027676, 4.620222222373953969, 0.2206173157302028787 ) ) ;
#15786 = CARTESIAN_POINT ( 'NONE',  ( 0.1167790944451422702, 4.627166666742533074, -0.2819296736111110979 ) ) ;
#15787 = EDGE_LOOP ( 'NONE', ( #14110, #6917, #12196, #5982 ) ) ;
#15788 = CARTESIAN_POINT ( 'NONE',  ( -0.1993543840281266910, 4.012583333409198261, -0.1993543840281266910 ) ) ;
#15789 = CIRCLE ( 'NONE', #8760, 0.4062499999999995004 ) ;
#15790 = ORIENTED_EDGE ( 'NONE', *, *, #3957, .T. ) ;
#15791 = ORIENTED_EDGE ( 'NONE', *, *, #21215, .T. ) ;
#15792 = CALENDAR_DATE ( 2026, 7, 10 ) ;
#15793 = DIRECTION ( 'NONE',  ( 0.000000000000000000, 0.000000000000000000, -1.000000000000000000 ) ) ;
#15794 = CARTESIAN_POINT ( 'NONE',  ( 0.1292346314604057300, 0.4520833333333329485, 0.3119999999999998885 ) ) ;
#15795 = CC_DESIGN_APPROVAL ( #4769, ( #6827 ) ) ;
#15796 = CARTESIAN_POINT ( 'NONE',  ( 0.1292346314604057023, 0.1118055554038226151, 0.3119999999999998885 ) ) ;
#15797 = CARTESIAN_POINT ( 'NONE',  ( 0.04953945640252711835, 5.131792726399142524, 0.3025406458412410182 ) ) ;
#15798 = CYLINDRICAL_SURFACE ( 'NONE', #22413, 0.01874999999999999584 ) ;
#15799 = CARTESIAN_POINT ( 'NONE',  ( -0.4687500000000004441, 0.08804416056838103299, 0.4143091105369764438 ) ) ;
#15800 = CLOSED_SHELL ( 'NONE', ( #874, #7129, #21535, #15373, #18396, #9429, #15925, #21950, #1398, #7828, #16348, #1843, #17651, #9525, #14525, #18640, #22417, #21397, #13024, #22286, #17495, #21158, #2702, #11385, #23341, #22156, #14226, #14282, #8098, #10929, #3814, #11277, #5589, #4482, #9999, #3614, #23592, #22535, #10974, #15432, #12190, #10275, #10372, #11975, #13664, #785, #4986, #22878, #8130, #23719, #22954, #10278, #12064, #12418, #4568, #14055, #21679, #966, #307, #526, #16783, #22597, #9070, #21511, #11451, #3569, #17849, #14868, #18873, #10022, #817, #7114, #18514, #9314, #9924, #4957, #1665, #21383, #15263, #6947 ) ) ;
#15801 = CARTESIAN_POINT ( 'NONE',  ( 0.000000000000000000, 5.384999999999999787, 0.000000000000000000 ) ) ;
#15802 = CARTESIAN_POINT ( 'NONE',  ( -0.2819296736111110979, 0.05972222214635559273, -0.1167790944451423396 ) ) ;
#15803 = CARTESIAN_POINT ( 'NONE',  ( 0.2764156081756483641, 0.1144950937579610056, 0.06402777777777945989 ) ) ;
#15804 = CARTESIAN_POINT ( 'NONE',  ( 0.000000000000000000, 0.1799999999999999933, 0.000000000000000000 ) ) ;
#15805 = CARTESIAN_POINT ( 'NONE',  ( -0.2819296736111110424, 4.467444444520308977, 0.1167790944451424923 ) ) ;
#15806 = CARTESIAN_POINT ( 'NONE',  ( 0.4500000000000003442, -0.2598076211353317344, 0.3779506566538943235 ) ) ;
#15807 = CARTESIAN_POINT ( 'NONE',  ( -0.3124999999999997224, -0.1294417382415924411, -0.04708333333333271364 ) ) ;
#15808 = CARTESIAN_POINT ( 'NONE',  ( -0.4645572405553155537, 0.2721000128023691178, 0.05892738626661214729 ) ) ;
#15809 = CARTESIAN_POINT ( 'NONE',  ( 0.2206173157302027954, 4.196611111111110404, -0.2206173157302028232 ) ) ;
#15810 = CARTESIAN_POINT ( 'NONE',  ( 0.2209708691207961651, 0.2209708691207959985, 0.1508333333333355120 ) ) ;
#15811 = CARTESIAN_POINT ( 'NONE',  ( 0.1869076612972776497, 4.966140514420732899, 0.2519720605836450744 ) ) ;
#15812 = LOCAL_TIME ( 21, 9, 13.00000000000000000, #15881 ) ;
#15813 = CARTESIAN_POINT ( 'NONE',  ( -1.399103805173478513E-17, 0.4635611116728546865, -1.084197934689580034 ) ) ;
#15814 = VERTEX_POINT ( 'NONE', #19727 ) ;
#15815 = CC_DESIGN_DATE_AND_TIME_ASSIGNMENT ( #13149, #6694, ( #12686 ) ) ;
#15816 = CARTESIAN_POINT ( 'NONE',  ( 0.000000000000000000, 0.000000000000000000, 0.000000000000000000 ) ) ;
#15817 = DESIGN_CONTEXT ( 'detailed design', #23355, 'design' ) ;
#15818 = CARTESIAN_POINT ( 'NONE',  ( 0.3065906244346884857, 4.142790625704452445, -0.06232558618896349295 ) ) ;
#15819 = CARTESIAN_POINT ( 'NONE',  ( -0.2230971623002953874, 0.2230971623002954152, 0.05881944444444627690 ) ) ;
#15820 = CARTESIAN_POINT ( 'NONE',  ( 0.2726203751773835227, 3.812261744675993214, -0.1571308155000509799 ) ) ;
#15821 = CC_DESIGN_SECURITY_CLASSIFICATION ( #6483, ( #24135 ) ) ;
#15822 = CARTESIAN_POINT ( 'NONE',  ( 0.2233192592356399997, 0.1473214284738861568, -0.3073725909049500049 ) ) ;
#15823 = CARTESIAN_POINT ( 'NONE',  ( 0.1167790944451423535, 0.09444444436857780956, 0.2819296736111110979 ) ) ;
#15824 = CARTESIAN_POINT ( 'NONE',  ( -0.2764156081756484196, -0.1144950937579609362, -0.01236111111111004406 ) ) ;
#15825 = CYLINDRICAL_SURFACE ( 'NONE', #24023, 0.3125000000000000000 ) ;
#15826 = CARTESIAN_POINT ( 'NONE',  ( -0.3023734573831343142, -0.03492818159267604278, -0.09342498493132676829 ) ) ;
#15827 = CARTESIAN_POINT ( 'NONE',  ( 0.1144950937579609085, -0.2764156081756484751, 0.4459722222222269328 ) ) ;
#15828 = ORIENTED_EDGE ( 'NONE', *, *, #8255, .F. ) ;
#15829 = CARTESIAN_POINT ( 'NONE',  ( 0.2206173157302027954, 3.863277777777777366, -0.2206173157302028232 ) ) ;
#15830 = LINE ( 'NONE', #3144, #10159 ) ;
#15831 = LINE ( 'NONE', #23250, #1657 ) ;
#15832 = CARTESIAN_POINT ( 'NONE',  ( 0.2206173157302028232, 0.4138888888888885287, -0.2206173157302028232 ) ) ;
#15833 = CARTESIAN_POINT ( 'NONE',  ( 0.3119999999999999996, 5.026472222222221120, -0.1292346314604056745 ) ) ;
#15834 = AXIS2_PLACEMENT_3D ( 'NONE', #1343, #18408, #22063 ) ;
#15835 = EDGE_CURVE ( 'NONE', #16983, #8442, #10477, .T. ) ;
#15836 = CARTESIAN_POINT ( 'NONE',  ( -0.1167790944451423535, 4.196611111186976828, 0.2819296736111110979 ) ) ;
#15837 = CARTESIAN_POINT ( 'NONE',  ( 0.1993543840281267465, 4.054250000075865223, 0.1993543840281266633 ) ) ;
#15838 = CARTESIAN_POINT ( 'NONE',  ( -0.2206173157302027954, 0.5874999998482670627, -0.2206173157302028232 ) ) ;
#15839 = CARTESIAN_POINT ( 'NONE',  ( -0.4581189881604794678, 0.2644951211353315235, 0.3941886329748526263 ) ) ;
#15840 = CARTESIAN_POINT ( 'NONE',  ( 0.3059321453971730609, 2.458266394542412508E-17, 0.1926420918000893712 ) ) ;
#15841 = EDGE_LOOP ( 'NONE', ( #20532, #5371, #15205, #10555 ) ) ;
#15842 = ORIENTED_EDGE ( 'NONE', *, *, #19903, .T. ) ;
#15843 = CARTESIAN_POINT ( 'NONE',  ( 0.3125000000000000000, -5.740531871003217465E-17, 0.09527777777777987622 ) ) ;
#15844 = CARTESIAN_POINT ( 'NONE',  ( -0.1167790944451423535, 4.418833333409198261, 0.2819296736111110424 ) ) ;
#15845 = EDGE_CURVE ( 'NONE', #12538, #10074, #5363, .T. ) ;
#15846 = CARTESIAN_POINT ( 'NONE',  ( 1.222470958122163998, 2.978485840173427324, -0.8773620042323713175 ) ) ;
#15847 = CARTESIAN_POINT ( 'NONE',  ( -0.2268203959220264077, 5.160927072947055549, 0.1963408053746545645 ) ) ;
#15848 = COORDINATED_UNIVERSAL_TIME_OFFSET ( 0, 0, .AHEAD. ) ;
#15849 = CARTESIAN_POINT ( 'NONE',  ( 0.1916493530484527641, 0.4197546306156790252, 0.4334994210334169318 ) ) ;
#15850 = CARTESIAN_POINT ( 'NONE',  ( -0.1144950937579609779, 0.2764156081756484196, 0.07791666666666847985 ) ) ;
#15851 = VECTOR ( 'NONE', #15893, 39.37007874015748143 ) ;
#15852 = CARTESIAN_POINT ( 'NONE',  ( -0.1993543840281266355, 3.984805555631421470, 0.1993543840281267465 ) ) ;
#15853 = CARTESIAN_POINT ( 'NONE',  ( -0.1292346314604056190, 0.3687499999999997446, -0.3119999999999999996 ) ) ;
#15854 = CARTESIAN_POINT ( 'NONE',  ( -0.2206173157302027676, 4.891055555555555046, 0.2206173157302028787 ) ) ;
#15855 = CARTESIAN_POINT ( 'NONE',  ( -0.1954553509668046640, 0.1954553509668046918, 0.2550000000000031686 ) ) ;
#15856 = CARTESIAN_POINT ( 'NONE',  ( -0.2923287055106771337, 0.1258928570453147211, 0.2123892367102619971 ) ) ;
#15857 = CARTESIAN_POINT ( 'NONE',  ( -0.1993543840281267465, 0.1256944443685777957, 0.1993543840281266633 ) ) ;
#15858 = CARTESIAN_POINT ( 'NONE',  ( -0.2209708691207961095, 0.2209708691207961373, -0.05055555555555459740 ) ) ;
#15859 = LINE ( 'NONE', #3053, #22469 ) ;
#15860 = CARTESIAN_POINT ( 'NONE',  ( 3.820898013339742174E-17, 5.384999999999999787, 0.3119999999999999996 ) ) ;
#15861 = CARTESIAN_POINT ( 'NONE',  ( 0.3999999999999999667, 0.3964285714285711859, 0.1299678784931626307 ) ) ;
#15862 = CARTESIAN_POINT ( 'NONE',  ( 0.3155070326520292845, -5.795770164686806123E-17, 0.3122916666666701313 ) ) ;
#15863 = DIRECTION ( 'NONE',  ( 0.000000000000000000, 0.000000000000000000, -1.000000000000000000 ) ) ;
#15864 = CARTESIAN_POINT ( 'NONE',  ( 1.679791495769851560E-14, 3.793833333485275183, 0.3119999999999999996 ) ) ;
#15865 = LINE ( 'NONE', #12583, #13279 ) ;
#15866 = CARTESIAN_POINT ( 'NONE',  ( -0.1993543840281266633, 0.5562499999241333759, -0.1993543840281266910 ) ) ;
#15867 = CARTESIAN_POINT ( 'NONE',  ( -0.2819296736111110979, 4.033416666742532186, 0.000000000000000000 ) ) ;
#15868 = CARTESIAN_POINT ( 'NONE',  ( 0.4000000000000000222, 0.4624999998049151850, 0.000000000000000000 ) ) ;
#15869 = CARTESIAN_POINT ( 'NONE',  ( 0.2819296736111110424, 4.731333333409200925, -0.1167790944451423396 ) ) ;
#15870 = CARTESIAN_POINT ( 'NONE',  ( 0.2871469936926860367, 5.133785134621813739, -0.1062893706155275259 ) ) ;
#15871 = CARTESIAN_POINT ( 'NONE',  ( 0.2824505285658038822, 5.074643056359858129, 0.1332943695421338060 ) ) ;
#15872 = ORIENTED_EDGE ( 'NONE', *, *, #11414, .T. ) ;
#15873 = AXIS2_PLACEMENT_3D ( 'NONE', #14071, #2970, #12497 ) ;
#15874 = CARTESIAN_POINT ( 'NONE',  ( 0.2206173157302027954, 4.807722222222221120, -0.2206173157302028232 ) ) ;
#15875 = CARTESIAN_POINT ( 'NONE',  ( -0.2206173157302028232, 3.884111111262842808, -0.2206173157302028232 ) ) ;
#15876 = EDGE_CURVE ( 'NONE', #11353, #12971, #8633, .T. ) ;
#15877 = CARTESIAN_POINT ( 'NONE',  ( 0.000000000000000000, 0.1799999999999999933, 0.000000000000000000 ) ) ;
#15878 = CARTESIAN_POINT ( 'NONE',  ( 0.000000000000000000, 0.000000000000000000, 0.000000000000000000 ) ) ;
#15879 = VERTEX_POINT ( 'NONE', #5206 ) ;
#15880 = CARTESIAN_POINT ( 'NONE',  ( -0.1167790944451423119, 4.842444444520309865, -0.2819296736111110979 ) ) ;
#15881 = COORDINATED_UNIVERSAL_TIME_OFFSET ( 0, 0, .AHEAD. ) ;
#15882 = CARTESIAN_POINT ( 'NONE',  ( 0.2703601470917495475, 2.740000000000000213, 0.1560925037015647998 ) ) ;
#15883 = ADVANCED_FACE ( 'NONE', ( #2901, #23490, #3145 ), #4847, .T. ) ;
#15884 = CARTESIAN_POINT ( 'NONE',  ( -1.853979398150703436E-06, 4.543833384706993606, -0.3119999999944916280 ) ) ;
#15885 = ORIENTED_EDGE ( 'NONE', *, *, #20049, .T. ) ;
#15886 = CARTESIAN_POINT ( 'NONE',  ( 1.726321361862525858E-17, 0.1187499999241333620, -0.2819296736111110979 ) ) ;
#15887 = AXIS2_PLACEMENT_3D ( 'NONE', #22194, #12958, #18420 ) ;
#15888 = DIRECTION ( 'NONE',  ( 0.000000000000000000, 0.000000000000000000, -1.000000000000000000 ) ) ;
#15889 = PLANE ( 'NONE',  #22833 ) ;
#15890 = CARTESIAN_POINT ( 'NONE',  ( -0.5116234456863466562, 0.6134519301839026495, 2.624425744575095809 ) ) ;
#15891 = CARTESIAN_POINT ( 'NONE',  ( -0.3613381517857144343, 0.2473214284738860791, 0.1174058825155740171 ) ) ;
#15892 = CARTESIAN_POINT ( 'NONE',  ( -0.2665248263244868743, 5.052834303660202586, -0.1630106687325746095 ) ) ;
#15893 = DIRECTION ( 'NONE',  ( -0.000000000000000000, -0.000000000000000000, 1.000000000000000000 ) ) ;
#15894 = CARTESIAN_POINT ( 'NONE',  ( 2.296137995767620676, 2.978485840173427324, -2.088288568297006265 ) ) ;
#15895 = CARTESIAN_POINT ( 'NONE',  ( -0.1167790944451423535, 3.807722222298087988, 0.2819296736111110424 ) ) ;
#15896 = CARTESIAN_POINT ( 'NONE',  ( 0.2828027056401378747, 5.033810059304799189, -0.1317826061406767446 ) ) ;
#15897 = CARTESIAN_POINT ( 'NONE',  ( 0.2730879860166738338, 1.999640111863030478, -2.842828497045944758 ) ) ;
#15898 = CARTESIAN_POINT ( 'NONE',  ( -0.1876242985175622935, 4.771710133335938409, -0.2524446861021691912 ) ) ;
#15899 = CARTESIAN_POINT ( 'NONE',  ( -1.910449006669871087E-17, 4.543833333485065573, -0.3119999999999999996 ) ) ;
#15900 = CARTESIAN_POINT ( 'NONE',  ( -1.726321361862525858E-17, 4.797305555631421470, -0.2819296736111110979 ) ) ;
#15901 = ORIENTED_EDGE ( 'NONE', *, *, #11798, .T. ) ;
#15902 = CARTESIAN_POINT ( 'NONE',  ( 0.2819296736111110979, 4.102861111186976828, -3.452642723725051716E-17 ) ) ;
#15903 = AXIS2_PLACEMENT_3D ( 'NONE', #18824, #9200, #3709 ) ;
#15904 = ORIENTED_EDGE ( 'NONE', *, *, #13957, .F. ) ;
#15905 = PERSON_AND_ORGANIZATION_ROLE ( 'design_owner' ) ;
#15906 = VERTEX_POINT ( 'NONE', #23729 ) ;
#15907 = CARTESIAN_POINT ( 'NONE',  ( 0.4687500000000022204, 0.2630304559196462444, 0.05971082423031254943 ) ) ;
#15908 = CARTESIAN_POINT ( 'NONE',  ( 1.910449006669871087E-17, 0.4763888888888885287, -0.3119999999999999996 ) ) ;
#15909 = DIRECTION ( 'NONE',  ( 0.000000000000000000, 0.9659258262890680902, 0.2588190451025215721 ) ) ;
#15910 = CARTESIAN_POINT ( 'NONE',  ( -0.1568165683378916209, 4.400276573276943104, 0.2727880797438460569 ) ) ;
#15911 = CARTESIAN_POINT ( 'NONE',  ( -0.4687500000000003886, -0.1752855097131576501, 0.4001617384052038595 ) ) ;
#15912 = CARTESIAN_POINT ( 'NONE',  ( 9.184120737366631376E-17, 0.1556215347031258134, -0.7500000000000001110 ) ) ;
#15913 = VECTOR ( 'NONE', #13358, 39.37007874015748143 ) ;
#15914 = CARTESIAN_POINT ( 'NONE',  ( 0.5997114317030027841, 2.978485840173427324, -1.206013144887902788 ) ) ;
#15915 = DIRECTION ( 'NONE',  ( 0.000000000000000000, 1.000000000000000000, 0.000000000000000000 ) ) ;
#15916 = CARTESIAN_POINT ( 'NONE',  ( 0.000000000000000000, 0.2764156081756484196, 0.07444444444444621445 ) ) ;
#15917 = EDGE_LOOP ( 'NONE', ( #8308, #16154, #13499, #22743 ) ) ;
#15918 = CARTESIAN_POINT ( 'NONE',  ( 0.000000000000000000, 5.384999999999999787, 0.000000000000000000 ) ) ;
#15919 = CARTESIAN_POINT ( 'NONE',  ( -0.1993543840281266910, 4.401472222298088433, -0.1993543840281266910 ) ) ;
#15920 = CARTESIAN_POINT ( 'NONE',  ( 0.1292346314604057300, 0.1743055555555551861, 0.3119999999999998885 ) ) ;
#15921 = CARTESIAN_POINT ( 'NONE',  ( -0.02089153872600517728, 0.7885332705621130867, -1.079944001585411373 ) ) ;
#15922 = LINE ( 'NONE', #16053, #118 ) ;
#15923 = CARTESIAN_POINT ( 'NONE',  ( 0.3119999999999998885, 0.4520833331816005995, 0.1292346314604058410 ) ) ;
#15924 = CARTESIAN_POINT ( 'NONE',  ( 0.2206173157302027954, 4.307722222222221120, -0.2206173157302028232 ) ) ;
#15925 = ADVANCED_FACE ( 'NONE', ( #8381 ), #10712, .F. ) ;
#15926 = CARTESIAN_POINT ( 'NONE',  ( -0.3119999999999999996, 5.113277777929509327, 0.000000000000000000 ) ) ;
#15927 = EDGE_CURVE ( 'NONE', #14781, #1954, #19955, .T. ) ;
#15928 = CARTESIAN_POINT ( 'NONE',  ( 0.1444491956679451461, 4.964733462867917169, 0.2770352471482286361 ) ) ;
#15929 = CARTESIAN_POINT ( 'NONE',  ( 0.2252755657635890640, 4.578756013223267196, 0.2171699826210613526 ) ) ;
#15930 = ORIENTED_EDGE ( 'NONE', *, *, #19953, .T. ) ;
#15931 = CARTESIAN_POINT ( 'NONE',  ( -0.5116234456863258950, 2.853030769935285260, -2.756251211572797288 ) ) ;
#15932 = AXIS2_PLACEMENT_3D ( 'NONE', #9968, #5931, #7648 ) ;
#15933 = CARTESIAN_POINT ( 'NONE',  ( 0.2032514787282173330, 4.133466838173744939, 0.2368180772981753890 ) ) ;
#15934 = CARTESIAN_POINT ( 'NONE',  ( 0.2230971623002953874, -0.2230971623002954429, 0.08659722222222429600 ) ) ;
#15935 = CARTESIAN_POINT ( 'NONE',  ( -0.2923287055106771337, 0.4116071427596003640, 0.2123892367102619971 ) ) ;
#15936 = CARTESIAN_POINT ( 'NONE',  ( 0.04084013455945455923, 3.794930617901433934, 0.3119999999999988338 ) ) ;
#15937 = PRODUCT_DEFINITION_SHAPE ( 'NONE', 'NONE',  #9710 ) ;
#15938 = CARTESIAN_POINT ( 'NONE',  ( -0.2233192592356399442, 0.1616071427596004473, -0.3073725909049500049 ) ) ;
#15939 = CARTESIAN_POINT ( 'NONE',  ( -0.1993543840281267465, 0.08402777770191115214, 0.1993543840281266633 ) ) ;
#15940 = CARTESIAN_POINT ( 'NONE',  ( -0.2764156081756484196, 1.692557448933383907E-17, 0.03972222222222369925 ) ) ;
#15941 = CARTESIAN_POINT ( 'NONE',  ( 0.000000000000000000, 3.700000000000000622, 0.000000000000000000 ) ) ;
#15942 = CARTESIAN_POINT ( 'NONE',  ( 5.178964085587577574E-17, 5.102861111186976828, 0.2819296736111110979 ) ) ;
#15943 = CARTESIAN_POINT ( 'NONE',  ( -0.2764156081756484196, 0.1144950937579609918, 0.4251388888888933959 ) ) ;
#15944 = ORIENTED_EDGE ( 'NONE', *, *, #20051, .F. ) ;
#15945 = DIRECTION ( 'NONE',  ( -1.000000000000000000, 1.224646799147353700E-16, 0.000000000000000000 ) ) ;
#15946 = CC_DESIGN_PERSON_AND_ORGANIZATION_ASSIGNMENT ( #20412, #5168, ( #13174 ) ) ;
#15947 = CARTESIAN_POINT ( 'NONE',  ( -0.1474229253358168013, 4.289503790139332473, 0.2774834428915729512 ) ) ;
#15948 = CARTESIAN_POINT ( 'NONE',  ( -0.4875000000000003220, 0.2598076211353315124, 0.06112444011295373181 ) ) ;
#15949 = CARTESIAN_POINT ( 'NONE',  ( -5.731347020009612645E-17, 0.5041666666666663188, 0.3119999999999999996 ) ) ;
#15950 = CARTESIAN_POINT ( 'NONE',  ( -0.1292346314604057023, 4.894527777777777366, 0.3119999999999998885 ) ) ;
#15951 = AXIS2_PLACEMENT_3D ( 'NONE', #4294, #2479, #15520 ) ;
#15952 = CARTESIAN_POINT ( 'NONE',  ( 0.2819296736111110979, 4.325083333409198261, -3.452642723725051716E-17 ) ) ;
#15953 = CARTESIAN_POINT ( 'NONE',  ( 5.178964085587577574E-17, 3.936194444520310309, 0.2819296736111110979 ) ) ;
#15954 = DIRECTION ( 'NONE',  ( 0.000000000000000000, 0.000000000000000000, 1.000000000000000000 ) ) ;
#15955 = CARTESIAN_POINT ( 'NONE',  ( -0.1292346314604081170, 3.873694444444442997, -0.3119999999999975016 ) ) ;
#15956 = FACE_OUTER_BOUND ( 'NONE', #12122, .T. ) ;
#15957 = ORIENTED_EDGE ( 'NONE', *, *, #20209, .F. ) ;
#15958 = ORIENTED_EDGE ( 'NONE', *, *, #13653, .F. ) ;
#15959 = CARTESIAN_POINT ( 'NONE',  ( 0.4593750000000003664, 0.2760455974562901482, 0.3779506566538943235 ) ) ;
#15960 = CARTESIAN_POINT ( 'NONE',  ( 0.1993543840281267465, 4.540361111186976828, 0.1993543840281266633 ) ) ;
#15961 = CARTESIAN_POINT ( 'NONE',  ( -0.2233192592356399442, 0.01874999990245759460, -0.3073725909049499494 ) ) ;
#15962 = EDGE_CURVE ( 'NONE', #19216, #8072, #15831, .T. ) ;
#15963 = CARTESIAN_POINT ( 'NONE',  ( 0.1292346314604131963, 3.790361111111110404, 0.3119999999999925611 ) ) ;
#15964 = DATE_AND_TIME ( #2029, #1750 ) ;
#15965 = CARTESIAN_POINT ( 'NONE',  ( -0.4687500000000003886, -0.1725638498522215902, 0.06591651963122398261 ) ) ;
#15966 = VECTOR ( 'NONE', #22400, 39.37007874015748143 ) ;
#15967 = EDGE_CURVE ( 'NONE', #9548, #5345, #7112, .T. ) ;
#15968 = CARTESIAN_POINT ( 'NONE',  ( 0.1954553509668046640, -0.1954553509668047195, 0.05361111111111271227 ) ) ;
#15969 = VECTOR ( 'NONE', #20630, 39.37007874015748143 ) ;
#15970 = CARTESIAN_POINT ( 'NONE',  ( 0.1993543840281267465, 4.165361111186976828, 0.1993543840281266633 ) ) ;
#15971 = DATE_AND_TIME ( #15738, #4914 ) ;
#15972 = CARTESIAN_POINT ( 'NONE',  ( -0.2952551624447684597, 4.838429752736293388, 0.1030155185898169040 ) ) ;
#15973 = FACE_OUTER_BOUND ( 'NONE', #18119, .T. ) ;
#15974 = CARTESIAN_POINT ( 'NONE',  ( -0.2764156081756484196, -0.1144950937579609362, 0.2654166666666699093 ) ) ;
#15975 = CARTESIAN_POINT ( 'NONE',  ( 0.1116596296178199860, 0.1687499999024575648, -0.3436530038418508792 ) ) ;
#15976 = CARTESIAN_POINT ( 'NONE',  ( 0.2819296736111110424, 0.1430555554796889284, 0.1167790944451424923 ) ) ;
#15977 = CARTESIAN_POINT ( 'NONE',  ( -0.1347750699935967023, 0.2587654721081596998, 0.4032729751179568445 ) ) ;
#15978 = DIRECTION ( 'NONE',  ( -0.8660254037844434816, -0.000000000000000000, -0.4999999999999916178 ) ) ;
#15979 = CARTESIAN_POINT ( 'NONE',  ( -7.726019084026502927E-17, 0.3821428571428569509, 0.4205848896953069405 ) ) ;
#15980 = CARTESIAN_POINT ( 'NONE',  ( 0.1306872919485614071, -0.3155070326520293955, 0.3018750000000033906 ) ) ;
#15981 = EDGE_CURVE ( 'NONE', #6154, #14487, #5085, .T. ) ;
#15982 = VERTEX_POINT ( 'NONE', #19974 ) ;
#15983 = CARTESIAN_POINT ( 'NONE',  ( -0.7171867353193159822, 1.999640111863030256, -2.958139940446594007 ) ) ;
#15984 = CARTESIAN_POINT ( 'NONE',  ( -0.01784808211855408791, 3.766536899369928637, -0.3115622909592437595 ) ) ;
#15985 = CARTESIAN_POINT ( 'NONE',  ( 0.4687500000000002776, 0.2598076211353320120, 0.3779506566538942125 ) ) ;
#15986 = CARTESIAN_POINT ( 'NONE',  ( -0.1993543840281266633, 0.3895833332574667462, -0.1993543840281266910 ) ) ;
#15987 = CARTESIAN_POINT ( 'NONE',  ( 0.1167790944451422702, 4.016055555631422358, -0.2819296736111110424 ) ) ;
#15988 = CARTESIAN_POINT ( 'NONE',  ( 0.2923287055106771337, -0.05267857152611381266, -0.2123892367102620249 ) ) ;
#15989 = VERTEX_POINT ( 'NONE', #12679 ) ;
#15990 = CARTESIAN_POINT ( 'NONE',  ( 0.1167790944451422702, 4.682722222298088433, -0.2819296736111110424 ) ) ;
#15991 = CARTESIAN_POINT ( 'NONE',  ( 0.2309745581487958610, 5.136678346995997124, -0.2008515164670272302 ) ) ;
#15992 =( BOUNDED_SURFACE ( )  B_SPLINE_SURFACE ( 3, 1, ( 
 ( #6040, #13507 ),
 ( #2991, #19687 ),
 ( #21762, #6762 ),
 ( #23329, #1282 ) ),
 .UNSPECIFIED., .F., .F., .F. ) 
 B_SPLINE_SURFACE_WITH_KNOTS ( ( 4, 4 ),
 ( 2, 2 ),
 ( 0.000000000000000000, 1.000000000000000000 ),
 ( 0.000000000000000000, 1.000000000000000000 ),
 .UNSPECIFIED. ) 
 GEOMETRIC_REPRESENTATION_ITEM ( )  RATIONAL_B_SPLINE_SURFACE ( (
 ( 1.000000000000000000, 1.000000000000000000),
 ( 0.3333333333333338144, 0.3333333333333338144),
 ( 0.3333333333333338144, 0.3333333333333338144),
 ( 1.000000000000000000, 1.000000000000000000) ) ) 
 REPRESENTATION_ITEM ( '' )  SURFACE ( )  );
#15993 = AXIS2_PLACEMENT_3D ( 'NONE', #3409, #22181, #10859 ) ;
#15994 = CARTESIAN_POINT ( 'NONE',  ( 0.06335377612981468731, 0.1607590812887311205, 0.3999999999999999667 ) ) ;
#15995 = VECTOR ( 'NONE', #15387, 39.37007874015748143 ) ;
#15996 = ORIENTED_EDGE ( 'NONE', *, *, #9220, .F. ) ;
#15997 = CARTESIAN_POINT ( 'NONE',  ( 0.1294417382415924134, 0.3124999999999999445, 0.3834722222222266552 ) ) ;
#15998 = CARTESIAN_POINT ( 'NONE',  ( 0.1993543840281267465, 5.095916666742532186, 0.1993543840281266633 ) ) ;
#15999 = DIRECTION ( 'NONE',  ( 0.000000000000000000, 0.000000000000000000, -1.000000000000000000 ) ) ;
#16000 = ORIENTED_EDGE ( 'NONE', *, *, #1259, .F. ) ;
#16001 = CARTESIAN_POINT ( 'NONE',  ( 2.040570600599760365, 0.000000000000000000, -2.386288568296997870 ) ) ;
#16002 = CARTESIAN_POINT ( 'NONE',  ( -0.2819296736111110424, 4.967444444520310753, 0.1167790944451424923 ) ) ;
#16003 = APPROVAL_STATUS ( 'not_yet_approved' ) ;
#16004 = EDGE_LOOP ( 'NONE', ( #3339, #2131, #19050, #14645 ) ) ;
#16005 = CARTESIAN_POINT ( 'NONE',  ( -0.1549461890638730299, 5.104977286800423286, -0.2696689821046959756 ) ) ;
#16006 = CARTESIAN_POINT ( 'NONE',  ( -5.731347020009612645E-17, 0.2194444442927115380, 0.3119999999999999996 ) ) ;
#16007 = ORIENTED_EDGE ( 'NONE', *, *, #21983, .T. ) ;
#16008 = CARTESIAN_POINT ( 'NONE',  ( 0.1993543840281266910, 0.3895833332574667462, -0.1993543840281266910 ) ) ;
#16009 = AXIS2_PLACEMENT_3D ( 'NONE', #22967, #21270, #10186 ) ;
#16010 = ORIENTED_EDGE ( 'NONE', *, *, #3068, .T. ) ;
#16011 = CYLINDRICAL_SURFACE ( 'NONE', #17921, 0.3119999999999999996 ) ;
#16012 = CARTESIAN_POINT ( 'NONE',  ( 4.898587196589413075E-17, 3.700000000000000622, 0.4000000000000000222 ) ) ;
#16013 = CARTESIAN_POINT ( 'NONE',  ( -0.5116234456863466562, 3.856336430858469999, 2.734122295721124640 ) ) ;
#16014 = CARTESIAN_POINT ( 'NONE',  ( -0.3613381517857144343, 0.3901785713310290116, 0.1174058825155740171 ) ) ;
#16015 = CARTESIAN_POINT ( 'NONE',  ( -0.1649367396721517220, 5.048643163735372141, -0.2662506188672706386 ) ) ;
#16016 = EDGE_CURVE ( 'NONE', #12281, #18643, #1441, .T. ) ;
#16017 = LINE ( 'NONE', #6622, #14312 ) ;
#16018 = CARTESIAN_POINT ( 'NONE',  ( -0.1993543840281266910, 4.637583333409199149, -0.1993543840281266910 ) ) ;
#16019 = CARTESIAN_POINT ( 'NONE',  ( 0.000000000000000000, 5.384999999999999787, 0.000000000000000000 ) ) ;
#16020 = CARTESIAN_POINT ( 'NONE',  ( 0.2819296736111110424, 3.884111111186976384, -0.1167790944451423396 ) ) ;
#16021 = CARTESIAN_POINT ( 'NONE',  ( -0.1516584850513022498, 0.04616102306513563541, -0.2545636604784221046 ) ) ;
#16022 = CARTESIAN_POINT ( 'NONE',  ( 0.2824852782387745620, 5.033831851842247573, -0.1324622426912574757 ) ) ;
#16023 = CYLINDRICAL_SURFACE ( 'NONE', #9378, 0.4000000000000000222 ) ;
#16024 = CYLINDRICAL_SURFACE ( 'NONE', #12080, 0.1874999999999998335 ) ;
#16025 = CARTESIAN_POINT ( 'NONE',  ( 0.3119999999999999996, 4.307722222373953969, -3.820898013339742174E-17 ) ) ;
#16026 = CARTESIAN_POINT ( 'NONE',  ( 0.2819296736111110979, 4.727861111186976828, -3.452642723725051716E-17 ) ) ;
#16027 = VERTEX_POINT ( 'NONE', #17783 ) ;
#16028 = ADVANCED_FACE ( 'NONE', ( #6560 ), #2783, .T. ) ;
#16029 = CARTESIAN_POINT ( 'NONE',  ( 0.1993543840281267465, 4.151472222298087544, 0.1993543840281266633 ) ) ;
#16030 = EDGE_LOOP ( 'NONE', ( #4473, #20245, #21690, #13826 ) ) ;
#16031 = ORIENTED_EDGE ( 'NONE', *, *, #6337, .F. ) ;
#16032 = EDGE_CURVE ( 'NONE', #16274, #10685, #11318, .T. ) ;
#16033 = EDGE_CURVE ( 'NONE', #21793, #13845, #22292, .T. ) ;
#16034 = ORIENTED_EDGE ( 'NONE', *, *, #3638, .F. ) ;
#16035 = DATE_TIME_ROLE ( 'creation_date' ) ;
#16036 = EDGE_LOOP ( 'NONE', ( #23422, #8785, #19059, #4888 ) ) ;
#16037 =( BOUNDED_CURVE ( )  B_SPLINE_CURVE ( 2, ( #21164, #1286, #13740, #17994, #17627, #8227, #19693, #4694, #8346 ),
 .UNSPECIFIED., .F., .F. ) 
 B_SPLINE_CURVE_WITH_KNOTS ( ( 3, 2, 2, 2, 3 ),
 ( 0.2291666666666666574, 0.2395833333333333426, 0.2500000000000000000, 0.2604166666666666852, 0.2708333333333333148 ),
 .UNSPECIFIED. ) 
 CURVE ( )  GEOMETRIC_REPRESENTATION_ITEM ( )  RATIONAL_B_SPLINE_CURVE ( ( 1.000000000000000000, 0.9238795325112867385, 1.000000000000000000, 0.9238795325112867385, 1.000000000000000000, 0.9238795325112867385, 1.000000000000000000, 0.9238795325112867385, 1.000000000000000000 ) ) 
 REPRESENTATION_ITEM ( '' )  );
#16038 = DIRECTION ( 'NONE',  ( -1.177540334020096294E-17, 0.2588190451025213501, -0.9659258262890682012 ) ) ;
#16039 = CARTESIAN_POINT ( 'NONE',  ( 2.911000000000000032, 2.740000000000000213, 0.000000000000000000 ) ) ;
#16040 = ORIENTED_EDGE ( 'NONE', *, *, #22827, .T. ) ;
#16041 = CARTESIAN_POINT ( 'NONE',  ( 0.1292346314604056745, 0.3548611109593781676, -0.3119999999999999996 ) ) ;
#16042 = CARTESIAN_POINT ( 'NONE',  ( -0.006901823634795379095, 4.377352498881602827, -0.3119347351468002572 ) ) ;
#16043 = CARTESIAN_POINT ( 'NONE',  ( -0.4687500000000004441, -0.2208948773569446300, 0.4011966096125590964 ) ) ;
#16044 = DIRECTION ( 'NONE',  ( -0.000000000000000000, -1.000000000000000000, -0.000000000000000000 ) ) ;
#16045 = EDGE_CURVE ( 'NONE', #16588, #1106, #17110, .T. ) ;
#16046 = ORIENTED_EDGE ( 'NONE', *, *, #9294, .F. ) ;
#16047 = CARTESIAN_POINT ( 'NONE',  ( -0.2764156081756484196, 0.1144950937579609918, 0.3626388888888929518 ) ) ;
#16048 = CARTESIAN_POINT ( 'NONE',  ( 0.2819296736111110979, 0.03541666659080003332, 0.000000000000000000 ) ) ;
#16049 = CARTESIAN_POINT ( 'NONE',  ( 0.1954553509668047195, 0.1954553509668046085, -0.04361111111111028865 ) ) ;
#16050 = CARTESIAN_POINT ( 'NONE',  ( 0.1993543840281266633, 4.554250000075866112, -0.1993543840281266910 ) ) ;
#16051 = CARTESIAN_POINT ( 'NONE',  ( 0.2365780681204331104, 0.1757304751630093809, -0.08326837151785088098 ) ) ;
#16052 = CARTESIAN_POINT ( 'NONE',  ( -0.2728196097062217662, 0.3240212061204770788, -1.173116651927777365 ) ) ;
#16053 = CARTESIAN_POINT ( 'NONE',  ( -0.009375000000000190473, 0.5358532185916217161, 0.4425000000000000044 ) ) ;
#16054 = CARTESIAN_POINT ( 'NONE',  ( 0.000000000000000000, 5.384999999999999787, 0.000000000000000000 ) ) ;
#16055 = CARTESIAN_POINT ( 'NONE',  ( -0.2206173157302027676, 4.002166666666665762, 0.2206173157302028787 ) ) ;
#16056 = CARTESIAN_POINT ( 'NONE',  ( 0.1292346314604056190, 5.095916666818398610, -0.3119999999999999996 ) ) ;
#16057 = CARTESIAN_POINT ( 'NONE',  ( 0.3072865194369331920, 4.976230144801160549, -0.06581296942666983729 ) ) ;
#16058 = EDGE_LOOP ( 'NONE', ( #13213, #23188, #19444, #4558 ) ) ;
#16059 = FACE_OUTER_BOUND ( 'NONE', #15174, .T. ) ;
#16060 = ORIENTED_EDGE ( 'NONE', *, *, #10375, .T. ) ;
#16061 = CARTESIAN_POINT ( 'NONE',  ( 0.000000000000000000, 0.3125000000000000000, 0.2202777777777809309 ) ) ;
#16062 = CARTESIAN_POINT ( 'NONE',  ( -0.2230971623002953874, 0.2230971623002954152, 0.1143750000000022804 ) ) ;
#16063 = DIRECTION ( 'NONE',  ( 0.000000000000000000, 0.000000000000000000, -1.000000000000000000 ) ) ;
#16064 = EDGE_CURVE ( 'NONE', #10194, #12509, #14116, .T. ) ;
#16065 = VECTOR ( 'NONE', #8875, 39.37007874015748143 ) ;
#16066 = FACE_BOUND ( 'NONE', #1973, .T. ) ;
#16067 = EDGE_CURVE ( 'NONE', #17157, #3183, #5459, .T. ) ;
#16068 = ORIENTED_EDGE ( 'NONE', *, *, #10414, .F. ) ;
#16069 = CARTESIAN_POINT ( 'NONE',  ( -0.2923287055106771337, 0.1651785713310290060, -0.2123892367102620804 ) ) ;
#16070 = CARTESIAN_POINT ( 'NONE',  ( 0.2819296736111110979, 0.1083333332574667046, -0.1167790944451422980 ) ) ;
#16071 = CARTESIAN_POINT ( 'NONE',  ( 0.2764156081756484196, -5.077672346800151106E-17, 0.06750000000000168365 ) ) ;
#16072 = DIRECTION ( 'NONE',  ( -0.4999999999999918954, -0.000000000000000000, -0.8660254037844432595 ) ) ;
#16073 = CARTESIAN_POINT ( 'NONE',  ( -0.2819296736111110979, 5.144527777853643791, 0.000000000000000000 ) ) ;
#16074 = CARTESIAN_POINT ( 'NONE',  ( -0.1954553509668046640, 0.1954553509668046918, 0.4772222222222271548 ) ) ;
#16075 = ORIENTED_EDGE ( 'NONE', *, *, #17520, .F. ) ;
#16076 = DIRECTION ( 'NONE',  ( 0.000000000000000000, 0.000000000000000000, -1.000000000000000000 ) ) ;
#16077 = CARTESIAN_POINT ( 'NONE',  ( -0.2525534724708262124, 4.285549707882127635, 0.1860445849415660324 ) ) ;
#16078 = CARTESIAN_POINT ( 'NONE',  ( 0.000000000000000000, 5.384999999999999787, -0.3119999999999999996 ) ) ;
#16079 = CARTESIAN_POINT ( 'NONE',  ( 0.3119999999999999996, 0.4659722222222220100, -0.1292346314604056468 ) ) ;
#16080 = CARTESIAN_POINT ( 'NONE',  ( -0.1292346314604056745, 4.818138888888888083, -0.3119999999999999996 ) ) ;
#16081 = CARTESIAN_POINT ( 'NONE',  ( 0.2819296736111111534, 4.154944444520310753, 0.1167790944451422563 ) ) ;
#16082 = CARTESIAN_POINT ( 'NONE',  ( -0.1993543840281266355, 3.929250000075865668, 0.1993543840281267465 ) ) ;
#16083 = DIRECTION ( 'NONE',  ( -0.000000000000000000, -1.000000000000000000, -0.000000000000000000 ) ) ;
#16084 = CARTESIAN_POINT ( 'NONE',  ( -0.3880456933851578194, 0.3172275918314566012, 0.4112725064128996966 ) ) ;
#16085 = ORIENTED_EDGE ( 'NONE', *, *, #17414, .F. ) ;
#16086 = ORIENTED_EDGE ( 'NONE', *, *, #479, .F. ) ;
#16087 = DIRECTION ( 'NONE',  ( -0.1969820554421523873, -0.5836931634044232320, 0.7877184527664194968 ) ) ;
#16088 = CARTESIAN_POINT ( 'NONE',  ( 0.1993543840281267465, 4.429250000075865223, 0.1993543840281266633 ) ) ;
#16089 = AXIS2_PLACEMENT_3D ( 'NONE', #12409, #8721, #16173 ) ;
#16090 = CARTESIAN_POINT ( 'NONE',  ( 5.731347020009612645E-17, 3.786888888888888527, 0.3119999999999999996 ) ) ;
#16091 = CALENDAR_DATE ( 2026, 7, 10 ) ;
#16092 = CARTESIAN_POINT ( 'NONE',  ( 0.2206173157302027676, 0.06666666666666633267, 0.2206173157302028787 ) ) ;
#16093 = CARTESIAN_POINT ( 'NONE',  ( 0.1144950937579609085, -0.2764156081756484751, 0.05013888888889045381 ) ) ;
#16094 = CARTESIAN_POINT ( 'NONE',  ( -0.2819296736111110424, 4.092444444520309865, 0.1167790944451424923 ) ) ;
#16095 = CARTESIAN_POINT ( 'NONE',  ( -0.008720534560302872079, 4.821864677000621491, -0.3118955259047569983 ) ) ;
#16096 = CYLINDRICAL_SURFACE ( 'NONE', #1935, 0.3119999999999999996 ) ;
#16097 = CARTESIAN_POINT ( 'NONE',  ( 0.1144950937579609085, -0.2764156081756484751, 0.2793055555555589708 ) ) ;
#16098 = CARTESIAN_POINT ( 'NONE',  ( 0.1116596296178199860, -0.04553571438325667436, -0.3436530038418508792 ) ) ;
#16099 = CARTESIAN_POINT ( 'NONE',  ( -0.1993543840281267465, 0.5840277777019110550, 0.1993543840281266633 ) ) ;
#16100 = CARTESIAN_POINT ( 'NONE',  ( -0.1976201361917970800, 0.2172293928240131011, 0.4047180943398852038 ) ) ;
#16101 = FACE_OUTER_BOUND ( 'NONE', #657, .T. ) ;
#16102 = CARTESIAN_POINT ( 'NONE',  ( -0.2105386197592548914, 0.3855283470628421694, -0.7198427731174872335 ) ) ;
#16103 = CARTESIAN_POINT ( 'NONE',  ( 0.2764156081756484196, -5.077672346800151106E-17, 0.1161111111111132049 ) ) ;
#16104 = CARTESIAN_POINT ( 'NONE',  ( -0.1306872919485614903, 0.3155070326520293400, 0.3296527777777813473 ) ) ;
#16105 = CIRCLE ( 'NONE', #16886, 0.6398935782932173577 ) ;
#16106 = EDGE_LOOP ( 'NONE', ( #23823, #20048, #15828, #19072, #6981, #20969 ) ) ;
#16107 = CARTESIAN_POINT ( 'NONE',  ( -0.06335377612981472895, 0.06254479576953017594, -0.3999999999999999667 ) ) ;
#16108 = CARTESIAN_POINT ( 'NONE',  ( 0.4587617856195390087, 0.1788014388648739572, 0.4163859416987428785 ) ) ;
#16109 = CARTESIAN_POINT ( 'NONE',  ( -0.1167790944451424368, 0.3513888888130222155, 0.2819296736111110424 ) ) ;
#16110 = CARTESIAN_POINT ( 'NONE',  ( 0.2819296736111110424, 4.120222222298087544, -0.1167790944451423396 ) ) ;
#16111 = CARTESIAN_POINT ( 'NONE',  ( -0.3613381517857143232, 0.04374999990245761333, -0.1174058825155741004 ) ) ;
#16112 = VERTEX_POINT ( 'NONE', #18627 ) ;
#16113 = CARTESIAN_POINT ( 'NONE',  ( 0.1993543840281266633, 4.679250000075866112, -0.1993543840281266910 ) ) ;
#16114 = PLANE ( 'NONE',  #14325 ) ;
#16115 = EDGE_CURVE ( 'NONE', #15714, #16753, #19963, .T. ) ;
#16116 = CARTESIAN_POINT ( 'NONE',  ( 0.2188935633852181206, 5.085427961609339853, -0.2224342940683537995 ) ) ;
#16117 = ORIENTED_EDGE ( 'NONE', *, *, #18095, .T. ) ;
#16118 = CARTESIAN_POINT ( 'NONE',  ( 0.2209708691207961651, 0.2209708691207959985, 0.3800000000000043898 ) ) ;
#16119 = CARTESIAN_POINT ( 'NONE',  ( 0.1988758185427091096, 3.704359862811034798, -0.2404005174681773382 ) ) ;
#16120 = B_SPLINE_CURVE_WITH_KNOTS ( 'NONE', 3,
 ( #35, #16987, #9311, #5651 ),
 .UNSPECIFIED., .F., .F.,
 ( 4, 4 ),
 ( 0.08935694927272852528, 0.1543853174178342336 ),
 .UNSPECIFIED. ) ;
#16121 = CARTESIAN_POINT ( 'NONE',  ( 0.1239654880878250376, 4.206901642129136754, -0.2877763507316923874 ) ) ;
#16122 = CC_DESIGN_PERSON_AND_ORGANIZATION_ASSIGNMENT ( #13942, #4419, ( #21185 ) ) ;
#16123 = VECTOR ( 'NONE', #1233, 39.37007874015748854 ) ;
#16124 = VERTEX_POINT ( 'NONE', #9364 ) ;
#16125 = CARTESIAN_POINT ( 'NONE',  ( 5.178964085587577574E-17, 4.977861111186976828, 0.2819296736111110979 ) ) ;
#16126 = APPROVAL_STATUS ( 'not_yet_approved' ) ;
#16127 = CARTESIAN_POINT ( 'NONE',  ( -0.2993836324830134732, 5.117341590464007162, 0.07846023516673897302 ) ) ;
#16128 = CARTESIAN_POINT ( 'NONE',  ( -0.05332960504393493423, 4.570127177272008012, 0.3074086044673321472 ) ) ;
#16129 = ORIENTED_EDGE ( 'NONE', *, *, #11289, .F. ) ;
#16130 = CARTESIAN_POINT ( 'NONE',  ( 0.1167790944451423535, 0.2055555554796889006, 0.2819296736111110424 ) ) ;
#16131 = EDGE_LOOP ( 'NONE', ( #4194, #18673, #3370, #12921 ) ) ;
#16132 = CARTESIAN_POINT ( 'NONE',  ( -0.1167790944451422702, 0.01111111103524448085, -0.2819296736111110424 ) ) ;
#16133 = CARTESIAN_POINT ( 'NONE',  ( -0.2780745499956817079, 5.202872933541006439, 0.05779310355066207688 ) ) ;
#16134 = CARTESIAN_POINT ( 'NONE',  ( -0.3999999999999999667, 0.07499999999999995559, -0.1299678784931626030 ) ) ;
#16135 = CARTESIAN_POINT ( 'NONE',  ( -0.2368628722706440370, 5.064021184620441041, 0.2033160227223854977 ) ) ;
#16136 =( BOUNDED_CURVE ( )  B_SPLINE_CURVE ( 2, ( #23908, #1616, #14796, #3682, #12854, #7228, #5264, #7344, #22211 ),
 .UNSPECIFIED., .F., .F. ) 
 B_SPLINE_CURVE_WITH_KNOTS ( ( 3, 2, 2, 2, 3 ),
 ( 0.5982142857142856984, 0.6026785714285713969, 0.6071428571428569843, 0.6116071428571427937, 0.6160714285714284921 ),
 .UNSPECIFIED. ) 
 CURVE ( )  GEOMETRIC_REPRESENTATION_ITEM ( )  RATIONAL_B_SPLINE_CURVE ( ( 1.000000000000000000, 0.9238795325112867385, 1.000000000000000000, 0.9238795325112867385, 1.000000000000000000, 0.9238795325112867385, 1.000000000000000000, 0.9238795325112886259, 0.9999999999999981126 ) ) 
 REPRESENTATION_ITEM ( '' )  );
#16137 = CARTESIAN_POINT ( 'NONE',  ( 0.000000000000000000, 6.000000000000000888, 0.000000000000000000 ) ) ;
#16138 = CARTESIAN_POINT ( 'NONE',  ( 0.000000000000000000, 0.04579999999999925103, 0.2500000000000000000 ) ) ;
#16139 = CARTESIAN_POINT ( 'NONE',  ( -0.2819296736111110424, 4.759111111186978604, 0.1167790944451424923 ) ) ;
#16140 = CARTESIAN_POINT ( 'NONE',  ( -0.1292346314604058410, 0.2715277776260448528, 0.3119999999999998885 ) ) ;
#16141 = CIRCLE ( 'NONE', #13417, 0.2500000000000000000 ) ;
#16142 = CARTESIAN_POINT ( 'NONE',  ( 0.1797087373818229139, 3.721720957026357191, -0.2172305470487487511 ) ) ;
#16143 = CARTESIAN_POINT ( 'NONE',  ( -0.3013616091699982680, 0.05241076192755348556, 0.02684792332517318622 ) ) ;
#16144 = ADVANCED_FACE ( 'NONE', ( #14979 ), #19178, .F. ) ;
#16145 = CARTESIAN_POINT ( 'NONE',  ( -0.3125000000000000000, 1.913510623667739771E-17, 0.1716666666666689933 ) ) ;
#16146 = CARTESIAN_POINT ( 'NONE',  ( -0.4723638629038571235, -0.2802187124228194826, 0.04193801346286257781 ) ) ;
#16147 = CARTESIAN_POINT ( 'NONE',  ( 0.3385998376278290256, 4.184039657745742702E-17, -0.1012499999999999928 ) ) ;
#16148 = ADVANCED_FACE ( 'NONE', ( #11075 ), #11013, .F. ) ;
#16149 = CARTESIAN_POINT ( 'NONE',  ( 0.3119999999999999996, 4.255638889040621820, -0.1292346314604056745 ) ) ;
#16150 = CARTESIAN_POINT ( 'NONE',  ( 0.1993543840281267465, 4.776472222298088433, 0.1993543840281266633 ) ) ;
#16151 = ORIENTED_EDGE ( 'NONE', *, *, #7036, .T. ) ;
#16152 = CARTESIAN_POINT ( 'NONE',  ( -0.2819296736111110424, 3.745222222298088433, 0.1167790944451424923 ) ) ;
#16153 = EDGE_CURVE ( 'NONE', #10527, #3971, #5147, .T. ) ;
#16154 = ORIENTED_EDGE ( 'NONE', *, *, #17169, .T. ) ;
#16155 = APPROVAL_DATE_TIME ( #2855, #3735 ) ;
#16156 = VECTOR ( 'NONE', #6215, 39.37007874015748143 ) ;
#16157 = CARTESIAN_POINT ( 'NONE',  ( 7.478516849590708700E-17, -0.5289902422706634910, 0.3941886329748525153 ) ) ;
#16158 = CARTESIAN_POINT ( 'NONE',  ( 0.1294417382415921358, -0.3125000000000002220, 0.2515277777777811807 ) ) ;
#16159 = ORIENTED_EDGE ( 'NONE', *, *, #12864, .F. ) ;
#16160 = CARTESIAN_POINT ( 'NONE',  ( 0.2206173157302028232, 0.2402777776260448528, -0.2206173157302028232 ) ) ;
#16161 = CARTESIAN_POINT ( 'NONE',  ( -0.2537383668351042565, 4.385579815452747887, -0.1818392428212168843 ) ) ;
#16162 = CARTESIAN_POINT ( 'NONE',  ( -0.4687499999999812372, -0.02254683357178352554, 0.4289648683083041036 ) ) ;
#16163 = CARTESIAN_POINT ( 'NONE',  ( 0.01427445631846820454, 0.5924045552181391727, -0.7500000000000002220 ) ) ;
#16164 = ORIENTED_EDGE ( 'NONE', *, *, #12026, .F. ) ;
#16165 = APPROVAL_PERSON_ORGANIZATION ( #15526, #22804, #19060 ) ;
#16166 = VERTEX_POINT ( 'NONE', #10838 ) ;
#16167 = CARTESIAN_POINT ( 'NONE',  ( -0.1167790944451422702, 0.3305555554796889561, -0.2819296736111110979 ) ) ;
#16168 = CARTESIAN_POINT ( 'NONE',  ( -0.2764156081756484196, 1.692557448933383907E-17, 0.1438888888888912032 ) ) ;
#16169 = EDGE_LOOP ( 'NONE', ( #7182, #21375, #7158 ) ) ;
#16170 = CARTESIAN_POINT ( 'NONE',  ( -0.1167790944451423257, 4.398000000075866112, -0.2819296736111110424 ) ) ;
#16171 = CARTESIAN_POINT ( 'NONE',  ( 0.2209708691207961095, -0.2209708691207961651, 0.4147222222222265442 ) ) ;
#16172 = EDGE_CURVE ( 'NONE', #11997, #22384, #20337, .T. ) ;
#16173 = DIRECTION ( 'NONE',  ( 0.000000000000000000, 0.000000000000000000, 1.000000000000000000 ) ) ;
#16174 = CARTESIAN_POINT ( 'NONE',  ( -0.3125000000000000000, 1.913510623667739771E-17, 0.4008333333333378712 ) ) ;
#16175 = EDGE_CURVE ( 'NONE', #17621, #23261, #16806, .T. ) ;
#16176 = CARTESIAN_POINT ( 'NONE',  ( -0.3119999999999998885, 3.998694444444443441, 0.1292346314604058410 ) ) ;
#16177 = EDGE_CURVE ( 'NONE', #3065, #14583, #23590, .T. ) ;
#16178 = CARTESIAN_POINT ( 'NONE',  ( 0.3119999999999999996, 5.033416666818398610, -0.1292346314604056745 ) ) ;
#16179 = VECTOR ( 'NONE', #4631, 39.37007874015748854 ) ;
#16180 = ORIENTED_EDGE ( 'NONE', *, *, #6342, .T. ) ;
#16181 = DIRECTION ( 'NONE',  ( -0.000000000000000000, -1.000000000000000000, -0.000000000000000000 ) ) ;
#16182 = ORIENTED_EDGE ( 'NONE', *, *, #6441, .T. ) ;
#16183 = EDGE_CURVE ( 'NONE', #12247, #10339, #5577, .T. ) ;
#16184 = B_SPLINE_CURVE_WITH_KNOTS ( 'NONE', 3,
 ( #22888, #338, #14986, #5710, #13172, #22656, #4237, #13531, #8011, #5944, #20946, #20585, #13402, #3883, #20825, #11326, #11690, #9860, #17289, #13646, #11206, #18756, #22532, #9491, #221, #7658, #19587, #8128, #820, #15929, #1060, #701, #21183, #12057, #19469, #15700 ),
 .UNSPECIFIED., .F., .F.,
 ( 4, 2, 2, 2, 2, 1, 1, 1, 2, 2, 1, 2, 2, 2, 2, 2, 2, 2, 2, 4 ),
 ( 0.4111882619051633325, 0.4135300815769560323, 0.4158719012487487876, 0.4182137209205414874, 0.4205555405923341872, 0.4207019043218212517, 0.4207750861865647840, 0.4208116771189365224, 0.4208208248520294847, 0.4208299725851223916, 0.4208482680513083163, 0.4211409955102825009, 0.4217264504282308701, 0.4228973602641276086, 0.4240682701000244026, 0.4252391799359211411, 0.4264100897718179350, 0.4275809996077146735, 0.4287519094436114675, 0.4299228192795082060 ),
 .UNSPECIFIED. ) ;
#16185 = LOCAL_TIME ( 21, 9, 13.00000000000000000, #14326 ) ;
#16186 = CARTESIAN_POINT ( 'NONE',  ( -0.08160653437250413311, 4.902727489126108118, 0.3038913141772855986 ) ) ;
#16187 = CARTESIAN_POINT ( 'NONE',  ( -3.863846776457871776E-17, -0.3155070326520292845, 0.2463194444444477549 ) ) ;
#16188 = CARTESIAN_POINT ( 'NONE',  ( 0.3613381517857143232, 0.4366071427596004417, 0.1174058825155742114 ) ) ;
#16189 = CIRCLE ( 'NONE', #3338, 0.01874999999999999931 ) ;
#16190 = CARTESIAN_POINT ( 'NONE',  ( -0.4593750000000004219, -0.2760455974562901482, 0.06112444011295364160 ) ) ;
#16191 = EDGE_CURVE ( 'NONE', #2780, #2366, #23929, .T. ) ;
#16192 = CARTESIAN_POINT ( 'NONE',  ( 0.3613381517857143232, 0.2758928570453146878, 0.1174058825155742114 ) ) ;
#16193 = CARTESIAN_POINT ( 'NONE',  ( 0.1993543840281266355, 0.1534722221463556135, 0.1993543840281267465 ) ) ;
#16194 = CARTESIAN_POINT ( 'NONE',  ( 0.000000000000000000, 0.2764156081756484196, 0.08138888888889070361 ) ) ;
#16195 = CARTESIAN_POINT ( 'NONE',  ( 0.1167790944451424368, 5.161888888964753619, 0.2819296736111110424 ) ) ;
#16196 = CARTESIAN_POINT ( 'NONE',  ( 0.2764156081756484196, -5.077672346800151106E-17, 0.3452777777777816803 ) ) ;
#16197 = ORIENTED_EDGE ( 'NONE', *, *, #342, .T. ) ;
#16198 = CARTESIAN_POINT ( 'NONE',  ( -0.2094324427062704830, 4.605912874362315002, -0.2317822580471521066 ) ) ;
#16199 = CARTESIAN_POINT ( 'NONE',  ( -0.05039085684935192683, 4.267471303508200364, -0.3086620900824355029 ) ) ;
#16200 = CC_DESIGN_SECURITY_CLASSIFICATION ( #11937, ( #24130 ) ) ;
#16201 = DIRECTION ( 'NONE',  ( -0.7071067811865435759, -8.268739551449322488E-15, -0.7071067811865513475 ) ) ;
#16202 = CARTESIAN_POINT ( 'NONE',  ( 1.787800077107233543, 2.476536290232589810, -1.974119177195009511 ) ) ;
#16203 = CARTESIAN_POINT ( 'NONE',  ( 0.2206173157302027954, 4.641055555555554157, -0.2206173157302028232 ) ) ;
#16204 = CARTESIAN_POINT ( 'NONE',  ( 0.1167790944451422702, 3.946611111186976828, -0.2819296736111110979 ) ) ;
#16205 = CARTESIAN_POINT ( 'NONE',  ( -0.1167790944451423535, 3.821611111186977272, 0.2819296736111110424 ) ) ;
#16206 = CARTESIAN_POINT ( 'NONE',  ( 0.6781417736264208074, 2.740000000000000213, 0.3915253355519352496 ) ) ;
#16207 = CARTESIAN_POINT ( 'NONE',  ( 0.1292346314604056745, 0.5215277776260448528, -0.3119999999999999996 ) ) ;
#16208 = ORIENTED_EDGE ( 'NONE', *, *, #2869, .F. ) ;
#16209 = EDGE_LOOP ( 'NONE', ( #18411, #11662, #12687, #16279, #16876 ) ) ;
#16210 = FACE_OUTER_BOUND ( 'NONE', #9094, .T. ) ;
#16211 = CARTESIAN_POINT ( 'NONE',  ( 0.2819296736111110424, 4.550777777853643791, -0.1167790944451423396 ) ) ;
#16212 = EDGE_CURVE ( 'NONE', #13263, #15341, #5293, .T. ) ;
#16213 = CARTESIAN_POINT ( 'NONE',  ( -0.04339772285640217109, 4.489528066591655708, -0.3091585257072999027 ) ) ;
#16214 = COORDINATED_UNIVERSAL_TIME_OFFSET ( 0, 0, .AHEAD. ) ;
#16215 = CARTESIAN_POINT ( 'NONE',  ( -0.1541993830833572054, -0.2301090524146454375, -0.06558227484231497761 ) ) ;
#16216 = CARTESIAN_POINT ( 'NONE',  ( 0.2764156081756483641, 0.1144950937579610056, 0.1195833333333354703 ) ) ;
#16217 = LOCAL_TIME ( 21, 9, 13.00000000000000000, #21343 ) ;
#16218 = CARTESIAN_POINT ( 'NONE',  ( 0.1167790944451424506, 4.050777777853643791, 0.2819296736111110424 ) ) ;
#16219 = FACE_OUTER_BOUND ( 'NONE', #296, .T. ) ;
#16220 = CARTESIAN_POINT ( 'NONE',  ( -0.4749999999999999778, 3.575000000000000622, 2.908536147974962357E-17 ) ) ;
#16221 = FACE_OUTER_BOUND ( 'NONE', #16663, .T. ) ;
#16222 = CARTESIAN_POINT ( 'NONE',  ( -6.979263641208234666E-17, 0.1366071427596003973, 0.3799334167787516425 ) ) ;
#16223 = AXIS2_PLACEMENT_3D ( 'NONE', #23192, #1255, #21615 ) ;
#16224 = CARTESIAN_POINT ( 'NONE',  ( 0.1993543840281266910, 0.09791666659080001944, -0.1993543840281266910 ) ) ;
#16225 = CARTESIAN_POINT ( 'NONE',  ( 0.4687500000000002776, 0.2598076211353319009, 0.06112444011295373875 ) ) ;
#16226 = CARTESIAN_POINT ( 'NONE',  ( 5.731347020009612645E-17, 4.064666666666665762, 0.3119999999999999996 ) ) ;
#16227 = CARTESIAN_POINT ( 'NONE',  ( -0.1290899616220235746, 0.5438854779856191479, -0.7388258714505984148 ) ) ;
#16228 = CARTESIAN_POINT ( 'NONE',  ( -0.1954553509668046918, -0.1954553509668046640, 0.09527777777777970969 ) ) ;
#16229 = CARTESIAN_POINT ( 'NONE',  ( -0.3155070326520293400, -0.1306872919485614626, 0.4546527777777822910 ) ) ;
#16230 = ORIENTED_EDGE ( 'NONE', *, *, #15876, .F. ) ;
#16231 = VERTEX_POINT ( 'NONE', #15457 ) ;
#16232 = B_SPLINE_CURVE_WITH_KNOTS ( 'NONE', 3,
 ( #608, #19140, #21091, #17073 ),
 .UNSPECIFIED., .F., .F.,
 ( 4, 4 ),
 ( 0.000000000000000000, 0.002245614500282211434 ),
 .UNSPECIFIED. ) ;
#16233 = CARTESIAN_POINT ( 'NONE',  ( -0.1571291654308913377, 3.844849430847837368, 0.2726213298963375276 ) ) ;
#16234 = CARTESIAN_POINT ( 'NONE',  ( -0.1993543840281267465, 0.5145833332574667462, 0.1993543840281266633 ) ) ;
#16235 = CARTESIAN_POINT ( 'NONE',  ( -0.1167790944451423257, 3.800777777853643347, -0.2819296736111110424 ) ) ;
#16236 = CARTESIAN_POINT ( 'NONE',  ( 0.3613381517857143232, 0.008035714188171890621, 0.1174058825155742114 ) ) ;
#16237 = CARTESIAN_POINT ( 'NONE',  ( -0.1167790944451423535, 4.321611111186976828, 0.2819296736111110424 ) ) ;
#16238 = CARTESIAN_POINT ( 'NONE',  ( -1.861236469537744314E-17, 5.143359825938298435, -0.3039629827691722741 ) ) ;
#16239 = CARTESIAN_POINT ( 'NONE',  ( -0.3119999999999998885, 4.387583333333331836, 0.1292346314604058410 ) ) ;
#16240 = ORIENTED_EDGE ( 'NONE', *, *, #13467, .T. ) ;
#16241 = CARTESIAN_POINT ( 'NONE',  ( -1.910449006669871087E-17, 4.703555555555555046, -0.3119999999999999996 ) ) ;
#16242 = CARTESIAN_POINT ( 'NONE',  ( -0.3119999999999999996, 3.724388889040620931, 0.000000000000000000 ) ) ;
#16243 = EDGE_CURVE ( 'NONE', #23449, #397, #15336, .T. ) ;
#16244 = CARTESIAN_POINT ( 'NONE',  ( 0.007906488776360224083, 4.210275811275788094, -0.3119139767300507793 ) ) ;
#16245 = AXIS2_PLACEMENT_3D ( 'NONE', #20359, #11096, #18527 ) ;
#16246 = DIRECTION ( 'NONE',  ( 0.000000000000000000, 0.000000000000000000, -1.000000000000000000 ) ) ;
#16247 = CARTESIAN_POINT ( 'NONE',  ( -1.726321361862525858E-17, 4.950083333409199149, -0.2819296736111110979 ) ) ;
#16248 = COORDINATED_UNIVERSAL_TIME_OFFSET ( 0, 0, .AHEAD. ) ;
#16249 = ORIENTED_EDGE ( 'NONE', *, *, #18910, .F. ) ;
#16250 = DIRECTION ( 'NONE',  ( -0.000000000000000000, -0.000000000000000000, -1.000000000000000000 ) ) ;
#16251 = CARTESIAN_POINT ( 'NONE',  ( -0.1535707713190125057, 4.548357062511502846, -0.2744944684223242781 ) ) ;
#16252 = ORIENTED_EDGE ( 'NONE', *, *, #22697, .F. ) ;
#16253 = CARTESIAN_POINT ( 'NONE',  ( -0.1167790944451424368, 0.1986111110352444808, 0.2819296736111110424 ) ) ;
#16254 = CARTESIAN_POINT ( 'NONE',  ( -0.2819296736111110979, 0.07708333325746669074, -3.452642723725051716E-17 ) ) ;
#16255 = CARTESIAN_POINT ( 'NONE',  ( -0.3096848393397610977, 4.725704742377146772, 0.04818851133790161972 ) ) ;
#16256 = CARTESIAN_POINT ( 'NONE',  ( 0.1797084794423411680, 3.735609856212664948, -0.2172307604343298448 ) ) ;
#16257 = CARTESIAN_POINT ( 'NONE',  ( 0.3999999999999999667, -0.02500000000000002220, -0.1299678784931625475 ) ) ;
#16258 = CARTESIAN_POINT ( 'NONE',  ( -0.3097076850518720170, 5.056434073990216049, -0.04707335161509815930 ) ) ;
#16259 = CARTESIAN_POINT ( 'NONE',  ( 0.1292346314604058410, 4.179249999999998799, 0.3119999999999998885 ) ) ;
#16260 = CARTESIAN_POINT ( 'NONE',  ( -3.268767525105149064E-07, 3.877166675600695722, -0.3119999999998287477 ) ) ;
#16261 = DIRECTION ( 'NONE',  ( -0.8660254037844434816, 0.000000000000000000, 0.4999999999999915068 ) ) ;
#16262 = CARTESIAN_POINT ( 'NONE',  ( -0.1167790944451423257, 4.523000000075867000, -0.2819296736111110424 ) ) ;
#16263 = VECTOR ( 'NONE', #6992, 39.37007874015748143 ) ;
#16264 = CARTESIAN_POINT ( 'NONE',  ( -0.2206173157302027954, 0.2541666665149337478, -0.2206173157302028232 ) ) ;
#16265 = CARTESIAN_POINT ( 'NONE',  ( -0.1993543840281266910, 5.193138888964755395, -0.1993543840281266910 ) ) ;
#16266 = CARTESIAN_POINT ( 'NONE',  ( -0.2445782993682861228, 0.05555107339308604231, 0.1825817229059248648 ) ) ;
#16267 = CARTESIAN_POINT ( 'NONE',  ( 0.3067602754552773425, 3.750577552586075836, 0.05698053772913803244 ) ) ;
#16268 = CARTESIAN_POINT ( 'NONE',  ( 0.000000000000000000, 3.700000000000000622, -0.4000000000000000222 ) ) ;
#16269 = CARTESIAN_POINT ( 'NONE',  ( -0.06335377612981472895, 0.1964733670030168189, -0.3999999999999999667 ) ) ;
#16270 = CARTESIAN_POINT ( 'NONE',  ( -0.1292346314604056745, 4.380638889040620931, -0.3119999999999999996 ) ) ;
#16271 = CARTESIAN_POINT ( 'NONE',  ( 0.2819296736111110979, 4.675777777853643791, -0.1167790944451423396 ) ) ;
#16272 = CARTESIAN_POINT ( 'NONE',  ( -0.1167790944451423257, 3.898000000075865668, -0.2819296736111110424 ) ) ;
#16273 = ORIENTED_EDGE ( 'NONE', *, *, #8397, .F. ) ;
#16274 = VERTEX_POINT ( 'NONE', #17165 ) ;
#16275 = AXIS2_PLACEMENT_3D ( 'NONE', #14953, #7622, #18602 ) ;
#16276 = DATE_TIME_ROLE ( 'classification_date' ) ;
#16277 = CARTESIAN_POINT ( 'NONE',  ( 0.000000000000000000, 5.580232050807569344, 0.2501339745962155581 ) ) ;
#16278 = DIRECTION ( 'NONE',  ( 0.000000000000000000, 0.000000000000000000, -1.000000000000000000 ) ) ;
#16279 = ORIENTED_EDGE ( 'NONE', *, *, #6901, .F. ) ;
#16280 = CARTESIAN_POINT ( 'NONE',  ( -0.2206173157302027954, 0.1986111109593781676, -0.2206173157302028232 ) ) ;
#16281 = B_SPLINE_CURVE_WITH_KNOTS ( 'NONE', 3,
 ( #857, #13058, #22296, #9381, #14633, #7310, #20113, #12571 ),
 .UNSPECIFIED., .F., .F.,
 ( 4, 2, 2, 4 ),
 ( 0.000000000000000000, 0.0004997454757086400214, 0.0007496182135629598153, 0.0009994909514172796092 ),
 .UNSPECIFIED. ) ;
#16282 = CARTESIAN_POINT ( 'NONE',  ( -1.292110690191215982E-05, 4.377167013980166388, -0.3120000000056822875 ) ) ;
#16283 = EDGE_CURVE ( 'NONE', #16613, #5468, #22764, .T. ) ;
#16284 = CARTESIAN_POINT ( 'NONE',  ( -0.07209992989303458388, 3.712509909146093356, -0.3042198929050881073 ) ) ;
#16285 = CARTESIAN_POINT ( 'NONE',  ( 0.000000000000000000, 6.000000000000000888, 0.000000000000000000 ) ) ;
#16286 = CARTESIAN_POINT ( 'NONE',  ( -0.4000000000000000222, 0.3678571428571427715, 0.1299678784931624920 ) ) ;
#16287 = VERTEX_POINT ( 'NONE', #20699 ) ;
#16288 = CARTESIAN_POINT ( 'NONE',  ( 0.4872114317030045716, 2.978485840173427324, -1.400868860739402422 ) ) ;
#16289 = CARTESIAN_POINT ( 'NONE',  ( 0.1167790944451423119, 0.2680555554796889561, -0.2819296736111110979 ) ) ;
#16290 = CARTESIAN_POINT ( 'NONE',  ( 0.000000000000000000, 0.2764156081756484196, 0.2966666666666702423 ) ) ;
#16291 = EDGE_CURVE ( 'NONE', #12271, #23979, #19107, .T. ) ;
#16292 = CARTESIAN_POINT ( 'NONE',  ( 0.2819296736111110979, 4.543833333409199149, 0.1167790944451422425 ) ) ;
#16293 = CARTESIAN_POINT ( 'NONE',  ( 0.2663714005177876265, 0.1275804160634896045, -0.08436226472404015353 ) ) ;
#16294 = DIRECTION ( 'NONE',  ( -0.000000000000000000, -0.000000000000000000, -1.000000000000000000 ) ) ;
#16295 = CARTESIAN_POINT ( 'NONE',  ( -0.04307916566617576992, 4.237087336754088440, 0.3090125702873792735 ) ) ;
#16296 = CARTESIAN_POINT ( 'NONE',  ( 0.1292346314604056190, 4.033416666666666650, -0.3119999999999999996 ) ) ;
#16297 = AXIS2_PLACEMENT_3D ( 'NONE', #6642, #21640, #10558 ) ;
#16298 = CARTESIAN_POINT ( 'NONE',  ( 0.1292346314604058410, 5.019527777929509327, 0.3119999999999998885 ) ) ;
#16299 = CARTESIAN_POINT ( 'NONE',  ( -0.2206173157302027676, 4.168833333333332725, 0.2206173157302028787 ) ) ;
#16300 = EDGE_LOOP ( 'NONE', ( #18262, #16995, #15609, #9033, #14425, #10795, #9195, #819, #20755, #13530, #2243 ) ) ;
#16301 = CARTESIAN_POINT ( 'NONE',  ( -0.08612638745143788577, 4.879649618296496350, -0.3001248726556640101 ) ) ;
#16302 = CARTESIAN_POINT ( 'NONE',  ( 0.1306872919485614071, -0.3155070326520293955, 0.3609027777777820134 ) ) ;
#16303 = CARTESIAN_POINT ( 'NONE',  ( 0.3613381517857143232, 0.4401785713310289450, 0.000000000000000000 ) ) ;
#16304 = ADVANCED_FACE ( 'NONE', ( #7884 ), #9853, .T. ) ;
#16305 = VECTOR ( 'NONE', #20806, 39.37007874015748143 ) ;
#16306 = ORIENTED_EDGE ( 'NONE', *, *, #16922, .T. ) ;
#16307 = CARTESIAN_POINT ( 'NONE',  ( 0.1236067977499789028, 0.02857142857142853584, 0.3804226065180614791 ) ) ;
#16308 = CARTESIAN_POINT ( 'NONE',  ( -0.3613381517857143232, 0.2401785713310289894, -0.1174058825155741004 ) ) ;
#16309 = CARTESIAN_POINT ( 'NONE',  ( 0.1167790944451423119, 0.2263888888130222710, -0.2819296736111110979 ) ) ;
#16310 = CARTESIAN_POINT ( 'NONE',  ( -0.2764156081756484196, -0.1144950937579609362, 0.3209722222222259891 ) ) ;
#16311 = CARTESIAN_POINT ( 'NONE',  ( 0.1993543840281266633, 5.234805555631421470, -0.1993543840281266910 ) ) ;
#16312 = DIRECTION ( 'NONE',  ( 0.000000000000000000, 0.000000000000000000, -1.000000000000000000 ) ) ;
#16313 = EDGE_CURVE ( 'NONE', #21333, #5171, #8005, .T. ) ;
#16314 = EDGE_LOOP ( 'NONE', ( #11180, #19496, #21837, #7781 ) ) ;
#16315 = CARTESIAN_POINT ( 'NONE',  ( -0.1811091878839710123, 4.604899780125036202, -0.2541407697476306127 ) ) ;
#16316 = CARTESIAN_POINT ( 'NONE',  ( 0.000000000000000000, 0.4202679491924311006, 0.2510000000000000009 ) ) ;
#16317 = DIRECTION ( 'NONE',  ( -0.000000000000000000, -1.000000000000000000, -0.000000000000000000 ) ) ;
#16318 = CARTESIAN_POINT ( 'NONE',  ( -0.1294417382415922191, 0.3125000000000000000, 0.3279166666666702423 ) ) ;
#16319 = CARTESIAN_POINT ( 'NONE',  ( -0.2206173157302027676, 4.724388888888888083, 0.2206173157302028787 ) ) ;
#16320 = CARTESIAN_POINT ( 'NONE',  ( 0.2819296736111110979, 4.102861111186976828, -3.452642723725051716E-17 ) ) ;
#16321 = CARTESIAN_POINT ( 'NONE',  ( -0.1993543840281266910, 3.859805555631421470, -0.1993543840281266910 ) ) ;
#16322 =( BOUNDED_CURVE ( )  B_SPLINE_CURVE ( 2, ( #13548, #17063, #5959 ),
 .UNSPECIFIED., .F., .T. ) 
 B_SPLINE_CURVE_WITH_KNOTS ( ( 3, 3 ),
 ( 0.000000000000000000, 0.005292957132939932544 ),
 .UNSPECIFIED. ) 
 CURVE ( )  GEOMETRIC_REPRESENTATION_ITEM ( )  RATIONAL_B_SPLINE_CURVE ( ( 1.000000000000000000, 0.4999999999999997780, 1.000000000000000000 ) ) 
 REPRESENTATION_ITEM ( '' )  );
#16323 = CARTESIAN_POINT ( 'NONE',  ( -0.06335377612981497875, 0.2054019386266730252, -0.3999999999999999667 ) ) ;
#16324 = DIRECTION ( 'NONE',  ( -0.000000000000000000, -1.000000000000000000, -0.000000000000000000 ) ) ;
#16325 =( BOUNDED_CURVE ( )  B_SPLINE_CURVE ( 2, ( #15105, #20823, #13169, #22653, #2049, #22285, #22528, #20703, #335 ),
 .UNSPECIFIED., .F., .T. ) 
 B_SPLINE_CURVE_WITH_KNOTS ( ( 3, 2, 2, 2, 3 ),
 ( 0.6696428571428570953, 0.6741071428571429047, 0.6785714285714286031, 0.6830357142857144126, 0.6875000000000001110 ),
 .UNSPECIFIED. ) 
 CURVE ( )  GEOMETRIC_REPRESENTATION_ITEM ( )  RATIONAL_B_SPLINE_CURVE ( ( 1.000000000000000000, 0.9238795325112867385, 1.000000000000000000, 0.9238795325112867385, 1.000000000000000000, 0.9238795325112867385, 1.000000000000000000, 0.9238795325112848511, 1.000000000000001998 ) ) 
 REPRESENTATION_ITEM ( '' )  );
#16326 = ORIENTED_EDGE ( 'NONE', *, *, #10608, .T. ) ;
#16327 = CONICAL_SURFACE ( 'NONE', #8923, 0.4625000000000000777, 0.7853981633974498333 ) ;
#16328 = CARTESIAN_POINT ( 'NONE',  ( 0.7108475124358382136, 4.111524471938507119, -3.019372695974962717 ) ) ;
#16329 = CARTESIAN_POINT ( 'NONE',  ( -0.1167790944451423535, 4.474388888964753619, 0.2819296736111110424 ) ) ;
#16330 = CARTESIAN_POINT ( 'NONE',  ( -0.1665361594110063848, 4.493262398435235561, -0.2674012144246484257 ) ) ;
#16331 = PERSON_AND_ORGANIZATION ( #15518, #2538 ) ;
#16332 = DIRECTION ( 'NONE',  ( 0.000000000000000000, 0.000000000000000000, -1.000000000000000000 ) ) ;
#16333 = CARTESIAN_POINT ( 'NONE',  ( -0.2764156081756484196, -0.1144950937579609362, 0.3140277777777815138 ) ) ;
#16334 = EDGE_CURVE ( 'NONE', #8315, #20541, #13639, .T. ) ;
#16335 = EDGE_CURVE ( 'NONE', #8085, #14094, #21129, .T. ) ;
#16336 = CARTESIAN_POINT ( 'NONE',  ( -0.1993543840281266910, 4.082027777853643791, -0.1993543840281266910 ) ) ;
#16337 = DIRECTION ( 'NONE',  ( -0.7071067811865484609, 0.000000000000000000, -0.7071067811865464625 ) ) ;
#16338 = CARTESIAN_POINT ( 'NONE',  ( 0.03980666169698005713, 5.161137237538360623, -0.2968008138702253329 ) ) ;
#16339 = CARTESIAN_POINT ( 'NONE',  ( 2.114905110478964667E-17, 0.5924045552181390617, -0.7500000000000001110 ) ) ;
#16340 = CARTESIAN_POINT ( 'NONE',  ( -0.3613381517857143232, -0.02410714295468525253, -4.425116109941954795E-17 ) ) ;
#16341 = AXIS2_PLACEMENT_3D ( 'NONE', #1451, #9006, #22048 ) ;
#16342 = CARTESIAN_POINT ( 'NONE',  ( 0.1993543840281266910, 0.3201388888130222710, -0.1993543840281266910 ) ) ;
#16343 = CARTESIAN_POINT ( 'NONE',  ( -0.02575435819785533778, 0.2888475187005544176, 0.4010461685168428270 ) ) ;
#16344 = CARTESIAN_POINT ( 'NONE',  ( 0.3119999999999999996, 0.5736111111111107386, 0.000000000000000000 ) ) ;
#16345 = LINE ( 'NONE', #23876, #21 ) ;
#16346 = CARTESIAN_POINT ( 'NONE',  ( 0.1144950937579609085, -0.2764156081756484751, -0.005416666666665539281 ) ) ;
#16347 = CARTESIAN_POINT ( 'NONE',  ( 0.1144950937579609085, -0.2764156081756484751, 0.05708333333333493603 ) ) ;
#16348 = ADVANCED_FACE ( 'NONE', ( #2647 ), #4466, .F. ) ;
#16349 = ORIENTED_EDGE ( 'NONE', *, *, #1357, .F. ) ;
#16350 = EDGE_LOOP ( 'NONE', ( #11641, #22887, #18581, #518 ) ) ;
#16351 = CARTESIAN_POINT ( 'NONE',  ( -0.4000000000000000222, 0.08214285714285710083, 0.1299678784931624920 ) ) ;
#16352 = CARTESIAN_POINT ( 'NONE',  ( -0.3124999999999997224, -0.1294417382415924411, 0.008472222222223286386 ) ) ;
#16353 = CARTESIAN_POINT ( 'NONE',  ( -0.1292346314604058410, 0.1118055555555552139, 0.3119999999999998885 ) ) ;
#16354 = CARTESIAN_POINT ( 'NONE',  ( -0.2819296736111110424, 3.863277777853644235, -0.1167790944451423119 ) ) ;
#16355 = CARTESIAN_POINT ( 'NONE',  ( -0.2923287055106771337, -0.01696428581182810383, 0.2123892367102619971 ) ) ;
#16356 = CARTESIAN_POINT ( 'NONE',  ( -0.2819296736111110979, 4.477861111186976828, 0.000000000000000000 ) ) ;
#16357 = PRODUCT_DEFINITION_SHAPE ( 'NONE', 'NONE',  #24130 ) ;
#16358 = CARTESIAN_POINT ( 'NONE',  ( 0.1865217406463640371, 5.123621613869084435, 0.2451376668825187843 ) ) ;
#16359 = CARTESIAN_POINT ( 'NONE',  ( 0.08808798601667688910, 4.111524471938507119, -3.348023836630494632 ) ) ;
#16360 = ORIENTED_EDGE ( 'NONE', *, *, #13051, .T. ) ;
#16361 = CARTESIAN_POINT ( 'NONE',  ( 0.2206173157302028787, 4.682722222222222008, 0.2206173157302027954 ) ) ;
#16362 = CARTESIAN_POINT ( 'NONE',  ( 0.2819296736111110424, 5.217444444520309865, -0.1167790944451423396 ) ) ;
#16363 = VECTOR ( 'NONE', #20059, 39.37007874015748854 ) ;
#16364 = CARTESIAN_POINT ( 'NONE',  ( 0.2328681059028355482, 4.203070697174108972, -0.2076452145264223170 ) ) ;
#16365 = CIRCLE ( 'NONE', #22594, 0.01875000000000000971 ) ;
#16366 =( NAMED_UNIT ( * ) SI_UNIT ( $, .STERADIAN. ) SOLID_ANGLE_UNIT ( ) );
#16367 = CARTESIAN_POINT ( 'NONE',  ( -0.1292346314604069513, 5.005638888888888083, 0.3119999999999986673 ) ) ;
#16368 = APPLICATION_CONTEXT ( 'configuration controlled 3d designs of mechanical parts and assemblies' ) ;
#16369 = CARTESIAN_POINT ( 'NONE',  ( -0.2819296736111110979, 4.908416666742532186, 0.000000000000000000 ) ) ;
#16370 = PERSON_AND_ORGANIZATION ( #16684, #19688 ) ;
#16371 = CARTESIAN_POINT ( 'NONE',  ( 5.731347020009612645E-17, 4.786888888888888083, 0.3119999999999999996 ) ) ;
#16372 = CARTESIAN_POINT ( 'NONE',  ( 0.3119999999999999996, 4.915361111111110404, -0.1292346314604056745 ) ) ;
#16373 = VERTEX_POINT ( 'NONE', #15693 ) ;
#16374 = CARTESIAN_POINT ( 'NONE',  ( 0.2819296736111110424, 0.2749999999241333204, -0.1167790944451423119 ) ) ;
#16375 = ORIENTED_EDGE ( 'NONE', *, *, #3957, .F. ) ;
#16376 = DIRECTION ( 'NONE',  ( -1.749783102806362652E-15, -0.9607689228305231754, -0.2773500981126138520 ) ) ;
#16377 = CARTESIAN_POINT ( 'NONE',  ( 3.062437355670495659E-17, 5.579732050807569621, 0.2499999999999999722 ) ) ;
#16378 = DIRECTION ( 'NONE',  ( -1.000000000000000000, 0.000000000000000000, 0.000000000000000000 ) ) ;
#16379 = CARTESIAN_POINT ( 'NONE',  ( -0.1236067977499789583, -0.007142857142857164318, -0.3804226065180614791 ) ) ;
#16380 = CARTESIAN_POINT ( 'NONE',  ( -0.1404473344439336469, 5.067469647815745049, 0.2805009585328055999 ) ) ;
#16381 = EDGE_CURVE ( 'NONE', #17621, #4265, #23107, .T. ) ;
#16382 = LINE ( 'NONE', #21976, #21942 ) ;
#16383 = AXIS2_PLACEMENT_3D ( 'NONE', #14365, #8379, #19973 ) ;
#16384 = CARTESIAN_POINT ( 'NONE',  ( -0.3084949655708456029, 3.892483775246653011, 0.05129296941314141767 ) ) ;
#16385 = DIRECTION ( 'NONE',  ( 0.000000000000000000, 0.000000000000000000, 1.000000000000000000 ) ) ;
#16386 = AXIS2_PLACEMENT_3D ( 'NONE', #5512, #10646, #3317 ) ;
#16387 = CARTESIAN_POINT ( 'NONE',  ( 0.2819296736111110979, 4.505638888964754507, -3.452642723725051716E-17 ) ) ;
#16388 = CARTESIAN_POINT ( 'NONE',  ( -0.1166234456863465552, 0.9548081934128058723, 2.526417548891521037 ) ) ;
#16389 = CARTESIAN_POINT ( 'NONE',  ( -0.1236067977499790416, 0.1553571426620580231, 0.3804226065180614236 ) ) ;
#16390 = CARTESIAN_POINT ( 'NONE',  ( 0.1993543840281267465, 4.998694444520309865, 0.1993543840281266633 ) ) ;
#16391 = CARTESIAN_POINT ( 'NONE',  ( -0.2611519554406496191, 0.05500242899132112839, 0.1578457353328193979 ) ) ;
#16392 = CARTESIAN_POINT ( 'NONE',  ( 0.08400942620796066074, 3.763674766651834425, -0.3008225317091856033 ) ) ;
#16393 = DIRECTION ( 'NONE',  ( 0.000000000000000000, -1.000000000000000000, 0.000000000000000000 ) ) ;
#16394 = CARTESIAN_POINT ( 'NONE',  ( -0.3838096539023497233, 0.3196732703672032772, 0.06591861138174955059 ) ) ;
#16395 = CARTESIAN_POINT ( 'NONE',  ( -0.2206173157302028232, 4.328555555707287894, -0.2206173157302028232 ) ) ;
#16396 = CARTESIAN_POINT ( 'NONE',  ( 0.1993543840281267465, 4.609805555631421470, 0.1993543840281266633 ) ) ;
#16397 = CARTESIAN_POINT ( 'NONE',  ( -0.2819296736111110979, 3.797305555631421470, 0.000000000000000000 ) ) ;
#16398 = ORIENTED_EDGE ( 'NONE', *, *, #23008, .F. ) ;
#16399 = ORIENTED_EDGE ( 'NONE', *, *, #10812, .F. ) ;
#16400 = ORIENTED_EDGE ( 'NONE', *, *, #16482, .F. ) ;
#16401 = COORDINATED_UNIVERSAL_TIME_OFFSET ( 0, 0, .AHEAD. ) ;
#16402 = CARTESIAN_POINT ( 'NONE',  ( 0.4593749999999910960, -0.2760455974562953108, 0.06112444011295854740 ) ) ;
#16403 = APPROVAL ( #21877, 'UNSPECIFIED' ) ;
#16404 = CARTESIAN_POINT ( 'NONE',  ( 0.05000000000000028727, 2.740000000000000213, 0.000000000000000000 ) ) ;
#16405 = DIRECTION ( 'NONE',  ( -0.000000000000000000, 1.000000000000000000, -0.000000000000000000 ) ) ;
#16406 = EDGE_LOOP ( 'NONE', ( #15650, #13377 ) ) ;
#16407 = CARTESIAN_POINT ( 'NONE',  ( -0.3119999999999999996, 0.2090277776260448250, 0.1292346314604056190 ) ) ;
#16408 = CARTESIAN_POINT ( 'NONE',  ( -0.03266130754527781649, 4.378054373819415090, -0.3103992783048078463 ) ) ;
#16409 = CARTESIAN_POINT ( 'NONE',  ( -0.2212700040550385772, 3.731355058608409880, 0.2247321557902158817 ) ) ;
#16410 = CARTESIAN_POINT ( 'NONE',  ( -0.2206173157302028787, 0.2749999999999996891, 0.2206173157302027954 ) ) ;
#16411 = CARTESIAN_POINT ( 'NONE',  ( 0.1884737858362492136, 0.4666198245431632530, -0.7259526178673825214 ) ) ;
#16412 = EDGE_LOOP ( 'NONE', ( #9007, #19478, #9348, #19176 ) ) ;
#16413 = ORIENTED_EDGE ( 'NONE', *, *, #12915, .T. ) ;
#16414 = EDGE_LOOP ( 'NONE', ( #19878, #10766, #5832, #14244, #12116 ) ) ;
#16415 = DIRECTION ( 'NONE',  ( -0.000000000000000000, 4.205955132072524856E-15, -1.000000000000000000 ) ) ;
#16416 = CARTESIAN_POINT ( 'NONE',  ( -0.2764156081756484196, 0.1144950937579609918, 0.1959722222222249899 ) ) ;
#16417 = CARTESIAN_POINT ( 'NONE',  ( 0.2819296736111110979, 4.325083333409198261, -3.452642723725051716E-17 ) ) ;
#16418 = CARTESIAN_POINT ( 'NONE',  ( -0.2819296736111110979, 5.016055555631420582, -0.1167790944451422980 ) ) ;
#16419 = CARTESIAN_POINT ( 'NONE',  ( 0.5755194329394802688, 2.762520450461519061, -0.7459121653754773318 ) ) ;
#16420 = CARTESIAN_POINT ( 'NONE',  ( -0.3084396050889865459, 4.225691337356074051, 0.04700294603068136401 ) ) ;
#16421 = CARTESIAN_POINT ( 'NONE',  ( -0.2206173157302027676, 4.057722222222221120, 0.2206173157302028787 ) ) ;
#16422 = VECTOR ( 'NONE', #16996, 39.37007874015748143 ) ;
#16423 = CARTESIAN_POINT ( 'NONE',  ( -0.2206173157302028232, 4.995222222373954857, -0.2206173157302028232 ) ) ;
#16424 = CARTESIAN_POINT ( 'NONE',  ( 0.2556300033343845146, 4.802328034493535291, 0.1804581348862814294 ) ) ;
#16425 = ORIENTED_EDGE ( 'NONE', *, *, #1177, .T. ) ;
#16426 = CARTESIAN_POINT ( 'NONE',  ( -0.2493665650958605817, 4.896940045553083820, 0.1919006865458766919 ) ) ;
#16427 = VERTEX_POINT ( 'NONE', #17037 ) ;
#16428 = ADVANCED_FACE ( 'NONE', ( #22649 ), #5937, .F. ) ;
#16429 = CARTESIAN_POINT ( 'NONE',  ( 0.1306872919485616846, 0.3155070326520292290, 0.1595138888888915640 ) ) ;
#16430 = CARTESIAN_POINT ( 'NONE',  ( -0.2819296736111110979, 5.241750000075865223, 0.000000000000000000 ) ) ;
#16431 = B_SPLINE_CURVE_WITH_KNOTS ( 'NONE', 3,
 ( #18210, #23919, #22103, #9182, #3567, #8815, #12619, #1505, #7355, #14685, #3448, #11139, #23675, #23556, #14805, #16625, #14558, #6870, #12985, #10654, #8940, #21981, #5275, #12745, #20160, #1625, #18085, #14313, #1385, #20282, #6995, #14439, #22222, #21747, #9059, #5032, #7238, #5398, #5521 ),
 .UNSPECIFIED., .F., .F.,
 ( 4, 2, 1, 1, 1, 1, 1, 2, 2, 2, 2, 2, 2, 2, 2, 2, 2, 2, 2, 2, 2, 4 ),
 ( 0.4477383270978809171, 0.4477425025345394549, 0.4477466779711979927, 0.4477550288445150128, 0.4477717305911491641, 0.4478051340844174111, 0.4478719410709538495, 0.4480055550440267820, 0.4482727829901727024, 0.4488072388824644876, 0.4498761506670480581, 0.4509450624516316286, 0.4520139742362151991, 0.4530828860207987696, 0.4541517978053823401, 0.4552207095899659106, 0.4562896213745494811, 0.4573585331591330516, 0.4584274449437166221, 0.4605652685128837631, 0.4627030920820509041, 0.4648409156512180451 ),
 .UNSPECIFIED. ) ;
#16432 = CARTESIAN_POINT ( 'NONE',  ( 0.2472135954999579721, 0.05357142857142854070, -0.3402603233408160732 ) ) ;
#16433 = CARTESIAN_POINT ( 'NONE',  ( -0.2233192592356399442, 0.3758928570453146656, -0.3073725909049500049 ) ) ;
#16434 = CARTESIAN_POINT ( 'NONE',  ( -5.178964085587577574E-17, 0.2020833332574667185, 0.2819296736111110979 ) ) ;
#16435 = CARTESIAN_POINT ( 'NONE',  ( 0.1144950937579609085, -0.2764156081756484751, 0.2237500000000028910 ) ) ;
#16436 = CARTESIAN_POINT ( 'NONE',  ( -0.1167790944451423257, 5.134111111186976828, -0.2819296736111110424 ) ) ;
#16437 = CARTESIAN_POINT ( 'NONE',  ( 1.241811370555571286E-09, 4.488277777895108400, -0.3119999999999999996 ) ) ;
#16438 = ORIENTED_EDGE ( 'NONE', *, *, #10578, .T. ) ;
#16439 = CARTESIAN_POINT ( 'NONE',  ( -0.1167790944451423257, 4.786888888964755395, -0.2819296736111110424 ) ) ;
#16440 = CARTESIAN_POINT ( 'NONE',  ( -0.1916867731382111140, 4.177017067639016368, 0.2495446019803314319 ) ) ;
#16441 = CARTESIAN_POINT ( 'NONE',  ( 0.001496851655420368583, 4.877126432010315149, -0.3119969275169424128 ) ) ;
#16442 = CARTESIAN_POINT ( 'NONE',  ( 0.000000000000000000, 5.580232050807569344, 0.000000000000000000 ) ) ;
#16443 = DIRECTION ( 'NONE',  ( 0.8660254037844434816, 0.000000000000000000, 0.4999999999999915068 ) ) ;
#16444 = CARTESIAN_POINT ( 'NONE',  ( 5.731347020009612645E-17, 4.675777777777777366, 0.3119999999999999996 ) ) ;
#16445 = CARTESIAN_POINT ( 'NONE',  ( 0.1993543840281267465, 3.984805555631421470, 0.1993543840281266633 ) ) ;
#16446 = CARTESIAN_POINT ( 'NONE',  ( -0.1167790944451423535, 3.766055555631421470, 0.2819296736111110424 ) ) ;
#16447 = CARTESIAN_POINT ( 'NONE',  ( 0.2967651801959635405, 4.032702029939365218, -0.09630854978782486808 ) ) ;
#16448 = CARTESIAN_POINT ( 'NONE',  ( 0.3119999999999999996, 0.5145833331816004330, -0.1292346314604056468 ) ) ;
#16449 = ORIENTED_EDGE ( 'NONE', *, *, #14975, .F. ) ;
#16450 = EDGE_CURVE ( 'NONE', #9622, #960, #9776, .T. ) ;
#16451 = CARTESIAN_POINT ( 'NONE',  ( -0.2819296736111110979, 4.352861111186976828, 0.000000000000000000 ) ) ;
#16452 = CARTESIAN_POINT ( 'NONE',  ( -0.3093573145567999894, 4.501048372529125707, -0.04052794418377673319 ) ) ;
#16453 = VECTOR ( 'NONE', #14342, 39.37007874015748143 ) ;
#16454 = EDGE_CURVE ( 'NONE', #9466, #431, #927, .T. ) ;
#16455 = FACE_OUTER_BOUND ( 'NONE', #22721, .T. ) ;
#16456 = CARTESIAN_POINT ( 'NONE',  ( -0.2764156081756484196, 1.692557448933383907E-17, 0.1438888888888912032 ) ) ;
#16457 = CARTESIAN_POINT ( 'NONE',  ( -0.08166535435460516024, 3.958181172869919440, 0.3038794725157443755 ) ) ;
#16458 = DIRECTION ( 'NONE',  ( 0.000000000000000000, 0.000000000000000000, 1.000000000000000000 ) ) ;
#16459 = CARTESIAN_POINT ( 'NONE',  ( 0.2764156081756484196, -5.077672346800151106E-17, 0.3452777777777816803 ) ) ;
#16460 = CARTESIAN_POINT ( 'NONE',  ( 0.1116596296178199027, 0.2116071427596004084, 0.3436530038418508792 ) ) ;
#16461 = CARTESIAN_POINT ( 'NONE',  ( -5.178964085587577574E-17, 0.3548611110352444808, 0.2819296736111110979 ) ) ;
#16462 = CARTESIAN_POINT ( 'NONE',  ( -0.4749999999999999778, 3.575000000000000622, 2.908536147974962357E-17 ) ) ;
#16463 = CARTESIAN_POINT ( 'NONE',  ( 0.000000000000000000, 0.1199999999999999678, 0.000000000000000000 ) ) ;
#16464 = CARTESIAN_POINT ( 'NONE',  ( 2.114905110478964667E-17, 0.5924045552181390617, -0.7500000000000001110 ) ) ;
#16465 = CARTESIAN_POINT ( 'NONE',  ( 0.1144950937579611444, 0.2764156081756483641, -0.08874999999999956535 ) ) ;
#16466 = B_SPLINE_CURVE_WITH_KNOTS ( 'NONE', 3,
 ( #4077, #2263, #11654, #6023, #13492, #20907, #19078, #6845, #16358, #23412, #1239, #1356, #6601, #10402, #19770, #3067, #6481, #2821, #14165, #12467, #23288, #14048, #21595, #4891, #1117, #17825, #2945, #15870, #21479, #3181, #4764, #15991, #19889, #18059, #6721, #12353, #10630, #17944, #12235, #10513, #6968, #8787, #16238 ),
 .UNSPECIFIED., .F., .F.,
 ( 4, 2, 2, 2, 2, 2, 2, 2, 2, 2, 2, 2, 1, 2, 2, 2, 2, 2, 2, 2, 2, 4 ),
 ( 0.04224588871235206156, 0.04377812836417232373, 0.04531036801599258590, 0.04684260766781284113, 0.04760872749372297569, 0.04837484731963310330, 0.04914096714554323092, 0.04990708697145335854, 0.05143932662327361377, 0.05297156627509387594, 0.05450380592691413117, 0.05526992575282425879, 0.05603604557873438641, 0.05680216540464452096, 0.05756828523055465552, 0.05910052488237491075, 0.06063276453419516598, 0.06216500418601542122, 0.06293112401192554883, 0.06369724383783567645, 0.06522948348965594556, 0.06676172314147620079 ),
 .UNSPECIFIED. ) ;
#16467 = VERTEX_POINT ( 'NONE', #1296 ) ;
#16468 = VERTEX_POINT ( 'NONE', #12172 ) ;
#16469 =( BOUNDED_CURVE ( )  B_SPLINE_CURVE ( 2, ( #21054, #2645, #6173, #10094, #4344, #17514, #19220, #7769, #2527 ),
 .UNSPECIFIED., .F., .T. ) 
 B_SPLINE_CURVE_WITH_KNOTS ( ( 3, 2, 2, 2, 3 ),
 ( 0.3958333333333333148, 0.4062500000000000000, 0.4166666666666666852, 0.4270833333333333148, 0.4375000000000000000 ),
 .UNSPECIFIED. ) 
 CURVE ( )  GEOMETRIC_REPRESENTATION_ITEM ( )  RATIONAL_B_SPLINE_CURVE ( ( 1.000000000000000000, 0.9238795325112867385, 1.000000000000000000, 0.9238795325112867385, 1.000000000000000000, 0.9238795325112867385, 1.000000000000000000, 0.9238795325112867385, 1.000000000000000000 ) ) 
 REPRESENTATION_ITEM ( '' )  );
#16470 = CARTESIAN_POINT ( 'NONE',  ( 0.000000000000000000, 0.05000000000000028727, -2.194053356329904947 ) ) ;
#16471 =( BOUNDED_SURFACE ( )  B_SPLINE_SURFACE ( 1, 2, ( 
 ( #16430, #1064, #12420, #12542, #8492, #19835, #9591, #10944, #7756, #22386, #5688, #9230, #16791, #16667, #15200, #9350, #20444, #17023, #20323, #18615, #196, #1667, #20684, #5803, #3741, #9469, #1785, #3861, #14852, #18372, #13030, #73, #13151, #18735, #18857, #317, #3610, #24090, #2032, #7402, #11063, #2156, #11187, #11304, #16548, #22267, #7638, #16903, #9100, #5445, #1906, #7516, #15087, #14965, #22509, #20564, #3492, #5564, #5323, #13268, #3975, #11425, #12788, #20206, #18492, #23970, #7282, #14731, #22147, #12909, #14612, #12797, #20455, #14861, #1794, #14976, #10956, #16679, #22036, #14742, #3504, #83, #7527, #12922, #3750, #210, #15097, #13277, #5332, #11436, #1917, #9360, #20333, #11194, #3622, #18867, #13038, #24101, #20696, #23980, #22278, #3872, #20216, #7649, #9480, #7410, #13161, #5454, #22398, #18502, #18381, #5574, #18623, #16803, #5698, #22520, #3986, #7292, #11072, #20575, #9238, #22157, #5813, #11315, #18746, #1676, #2042, #16913, #8996, #9109, #16559, #16439, #23849, #7169, #13519, #22761, #11563, #18991, #22992, #2289, #11680, #8115, #13749, #19103, #8002, #15569, #13636, #450, #9850, #2644, #6296, #691, #9971, #17513, #21053, #8236, #22877, #2409, #20935, #23104, #17034, #15454, #808, #15690, #10093, #21294, #17279, #19219, #7881, #328, #4228, #15333, #567, #6053, #6172, #20814, #6413, #13392, #21173, #4343, #11795, #2526, #4104, #13867, #9724, #4463, #17160, #17398, #11927, #4588, #19346, #2170, #12047, #9603, #7768, #15211, #22646, #5934, #16050, #10686, #4701, #16292, #19460, #18120, #8719, #924, #23223, #6774, #1171, #12286, #1294, #21412, #3003, #8354, #1050, #13985, #10571, #18002, #23342, #14218, #1417, #8846, #23705, #15805, #21892, #12406, #19825, #6653, #21655, #14100, #5181, #23465, #10452, #7026, #10329, #8609, #14340, #6532, #14468, #19948, #17879, #23585, #15919, #16170, #4816, #12169, #4942, #3120, #6902, #21773, #2758, #10209, #17756, #21527, #5060, #19700, #8477, #17635, #12529, #3238, #19578, #2870, #7502, #16771, #16417, #12772, #3596, #11048, #7268, #23954, #9086, #22011, #5309, #9335, #20190, #22129, #18600, #55, #5430, #18477, #1892, #24075, #10930, #20312, #13136, #14950, #11172, #20429, #3845, #7384, #18718, #9215, #12896, #14716, #9453, #3358, #1770, #11290, #2017, #20549, #7620, #16654, #5549, #18358, #10810, #14835, #1651, #22253, #16535, #13014, #3725, #18238, #20070, #22369, #5671, #16887, #180, #15071, #22493, #12652, #1537, #8968, #23826, #7148, #14588, #3479, #17370, #22621, #18962, #17135, #21145, #4316, #17253, #780, #5907, #8210, #4434, #22965, #20905, #20667, #2618, #300, #422, #17484, #8088, #9574, #539, #13609, #20785, #4200, #7974, #2501, #9820, #9940, #15425, #661, #11652, #3962, #22734, #15659, #7856, #15540, #2384, #11900, #13490, #4075, #15305, #11531, #17007, #6266, #21024, #5788, #11406, #13724, #11771, #2261, #19076, #7740, #18839, #22853, #19319, #6021, #13364, #10061, #2135, #15184, #9695, #6142, #19191, #13252, #2843, #16020, #4918, #14073, #1021, #6510, #8583, #23437, #12501, #18086, #21501, #2733, #21268, #10184, #4790, #23557, #17975, #19922, #8452, #21625, #8330, #12257, #4560, #15895, #12020, #3096, #23317, #6747, #8816, #6625, #17853, #1266, #23199, #10304, #19672, #2973, #23078, #19433, #10428, #12382, #15780, #1144, #1386, #5033, #14192, #19798, #10541, #8692, #16142 ),
 ( #6871, #14314, #4677, #17607, #17726, #12145, #21748, #19553, #3209, #898, #10655, #13958, #6387, #21387, #13835, #3694, #18686, #11022, #16265, #9183, #12865, #7473, #25, #1626, #24046, #20283, #14921, #1506, #13107, #23676, #22340, #5522, #21864, #20039, #3568, #22104, #9060, #22223, #18212, #23921, #5155, #21984, #10785, #7356, #14806, #20161, #18446, #5643, #20520, #3818, #12621, #1988, #16627, #12986, #3449, #1743, #10900, #6996, #20401, #7240, #11261, #7119, #5399, #11140, #3327, #14440, #16743, #14686, #18570, #12746, #1860, #16507, #8941, #9302, #16390, #23798, #14559, #5276, #18330, #7712, #13336, #6115, #20758, #15158, #6237, #17104, #7942, #20636, #4048, #4289, #13584, #13225, #9544, #392, #7831, #11503, #18937, #5876, #18807, #2103, #20995, #16977, #2234, #15398, #11746, #9667, #15277, #22824, #20877, #22590, #22704, #9911, #5994, #17228, #13460, #635, #272, #13702, #9424, #8066, #19167, #15043, #3937, #4171, #11623, #19053, #2476, #11379, #2354, #22465, #9795, #510, #17343, #15516, #22940, #21119, #4409, #11873, #19288, #5765, #16863, #148, #7592, #6480, #14047, #13932, #5005, #6600, #17700, #14284, #17582, #15869, #21594, #23054, #17943, #3066, #993, #6720, #23170, #1116, #12117, #8181, #10277, #21478, #2944, #15990, #16113, #6844, #873, #21362, #23411, #4649, #8304, #23526, #8422, #8549, #13808, #19526, #4889, #14164, #6362, #2706, #23287, #4763, #2820, #12234, #19645, #11995, #19409, #12352, #10157, #10401, #19769, #10512, #17824, #1238, #8664, #21721, #15756, #12466, #2592, #10038, #17460, #753, #15636, #21245, #4533, #16476, #5244, #7088, #16713, #10629, #9034, #18538, #1828, #3661, #14892, #20130, #12835, #1476, #18058, #14529, #8914, #3421, #16356, #10871, #14408, #14681, #6967, #24016, #3296, #12589, #7326, #22311, #14652, #19888, #20253, #23888, #11107, #9272, #7444, #21831, #21951, #5609, #22193, #23648, #22073, #3540, #10751, #18300, #7207, #16596, #5368, #14778, #10993, #5491, #1599, #1354, #12716, #3180, #18419, #12957, #1712, #8786, #9151, #18182, #20371, #23767, #5123, #16237, #20010, #22910, #3785, #7912, #4137, #11348, #2205, #16835, #11229, #22673, #15363, #245, #5734, #22792, #1950, #15013, #18776, #17066, #7679, #15129, #16945, #5963, #19024, #4021, #22556, #20608, #13425, #20846, #2439, #8034, #11470, #119, #18657, #7561, #18903, #13552, #6086, #9882, #5847, #11593, #22435, #9636, #9395, #13309, #13193, #17194, #20724, #2320, #13073, #360, #7801, #20966, #3905, #15244, #9756, #480, #20489, #2072, #4261, #11711, #9513, #19134, #15484, #17309, #602, #842, #11963, #19492, #17549, #4375, #13671, #15722, #8271, #4617, #12082, #954, #15837, #19377, #17669, #19611, #23134, #14015, #12203, #1080, #17788, #23025, #2674, #6447, #21561, #4731, #8385, #1206, #6326, #8637, #4851, #23378, #21328, #21085, #8151, #10125, #10240, #13900, #2787, #23256, #6565, #2905, #21445, #10364, #13778, #8512, #15953, #19732, #16082, #6686, #10006, #11835, #17429, #14131, #12319, #3034, #10481, #17913, #6206, #15603, #19253, #2558, #722, #21206, #4498, #23734, #23857, #9246, #16321, #18270, #18388, #23619, #3266, #12683, #20101, #23495, #19853, #7058, #5340, #16205, #5210, #18509, #5465, #21920, #18151, #5090, #3390, #10717, #21687, #6810, #8880, #1446, #10842, #1567, #9002, #16446, #12558, #7178, #12804, #14497, #14619, #20223, #1683, #10963, #6933 ) ),
 .UNSPECIFIED., .F., .F., .F. ) 
 B_SPLINE_SURFACE_WITH_KNOTS ( ( 2, 2 ),
 ( 3, 2, 2, 2, 2, 2, 2, 2, 2, 2, 2, 2, 2, 2, 2, 2, 2, 2, 2, 2, 2, 2, 2, 2, 2, 2, 2, 2, 2, 2, 2, 2, 2, 2, 2, 2, 2, 2, 2, 2, 2, 2, 2, 2, 2, 2, 2, 2, 2, 2, 2, 2, 2, 2, 2, 2, 2, 2, 2, 2, 2, 2, 2, 2, 2, 2, 2, 2, 2, 2, 2, 2, 2, 2, 2, 2, 2, 2, 2, 2, 2, 2, 2, 2, 2, 2, 2, 2, 2, 2, 2, 2, 2, 2, 2, 2, 2, 2, 2, 2, 2, 2, 2, 2, 2, 2, 2, 2, 2, 2, 2, 2, 2, 2, 2, 2, 2, 2, 2, 2, 2, 2, 2, 2, 2, 2, 2, 2, 2, 2, 2, 2, 2, 2, 2, 2, 2, 2, 2, 2, 2, 2, 2, 2, 2, 2, 2, 2, 2, 2, 2, 2, 2, 2, 2, 2, 2, 2, 2, 2, 2, 2, 2, 2, 2, 2, 2, 2, 2, 2, 2, 2, 2, 2, 2, 2, 2, 2, 2, 2, 2, 2, 2, 2, 2, 2, 2, 2, 2, 2, 2, 2, 2, 2, 2, 2, 2, 2, 2, 2, 2, 2, 2, 2, 2, 2, 2, 2, 2, 2, 2, 2, 2, 2, 2, 2, 2, 2, 2, 3 ),
 ( 0.000000000000000000, 1.000000000000000000 ),
 ( 0.000000000000000000, 0.004464285714285714038, 0.008928571428571428076, 0.01339285714285714211, 0.01785714285714285615, 0.02232142857142857192, 0.02678571428571428423, 0.03125000000000000000, 0.03571428571428571230, 0.04017857142857143155, 0.04464285714285714385, 0.04910714285714285615, 0.05357142857142856845, 0.05803571428571428770, 0.06250000000000000000, 0.06696428571428571230, 0.07142857142857142461, 0.07589285714285713691, 0.08035714285714286309, 0.08482142857142857539, 0.08928571428571428770, 0.09375000000000000000, 0.09821428571428571230, 0.1026785714285714246, 0.1071428571428571369, 0.1116071428571428631, 0.1160714285714285754, 0.1205357142857142877, 0.1250000000000000000, 0.1294642857142857262, 0.1339285714285714246, 0.1383928571428571508, 0.1428571428571428492, 0.1473214285714285754, 0.1517857142857142738, 0.1562500000000000000, 0.1607142857142857262, 0.1651785714285714246, 0.1696428571428571508, 0.1741071428571428492, 0.1785714285714285754, 0.1830357142857142738, 0.1875000000000000000, 0.1919642857142857262, 0.1964285714285714246, 0.2008928571428571508, 0.2053571428571428492, 0.2098214285714285754, 0.2142857142857142738, 0.2187500000000000000, 0.2232142857142857262, 0.2276785714285714246, 0.2321428571428571508, 0.2366071428571428492, 0.2410714285714285754, 0.2455357142857142738, 0.2500000000000000000, 0.2544642857142856984, 0.2589285714285714524, 0.2633928571428571508, 0.2678571428571428492, 0.2723214285714285476, 0.2767857142857143016, 0.2812500000000000000, 0.2857142857142856984, 0.2901785714285714524, 0.2946428571428571508, 0.2991071428571428492, 0.3035714285714285476, 0.3080357142857143016, 0.3125000000000000000, 0.3169642857142856984, 0.3214285714285714524, 0.3258928571428571508, 0.3303571428571428492, 0.3348214285714285476, 0.3392857142857143016, 0.3437500000000000000, 0.3482142857142856984, 0.3526785714285714524, 0.3571428571428571508, 0.3616071428571428492, 0.3660714285714285476, 0.3705357142857143016, 0.3750000000000000000, 0.3794642857142856984, 0.3839285714285714524, 0.3883928571428571508, 0.3928571428571428492, 0.3973214285714285476, 0.4017857142857143016, 0.4062500000000000000, 0.4107142857142856984, 0.4151785714285714524, 0.4196428571428571508, 0.4241071428571428492, 0.4285714285714285476, 0.4330357142857143016, 0.4375000000000000000, 0.4419642857142856984, 0.4464285714285714524, 0.4508928571428571508, 0.4553571428571428492, 0.4598214285714285476, 0.4642857142857143016, 0.4687500000000000000, 0.4732142857142856984, 0.4776785714285714524, 0.4821428571428571508, 0.4866071428571428492, 0.4910714285714285476, 0.4955357142857143016, 0.5000000000000000000, 0.5044642857142856984, 0.5089285714285713969, 0.5133928571428570953, 0.5178571428571429047, 0.5223214285714286031, 0.5267857142857143016, 0.5312500000000000000, 0.5357142857142856984, 0.5401785714285713969, 0.5446428571428570953, 0.5491071428571429047, 0.5535714285714286031, 0.5580357142857143016, 0.5625000000000000000, 0.5669642857142856984, 0.5714285714285713969, 0.5758928571428570953, 0.5803571428571429047, 0.5848214285714286031, 0.5892857142857143016, 0.5937500000000000000, 0.5982142857142856984, 0.6026785714285713969, 0.6071428571428570953, 0.6116071428571429047, 0.6160714285714286031, 0.6205357142857143016, 0.6250000000000000000, 0.6294642857142856984, 0.6339285714285713969, 0.6383928571428570953, 0.6428571428571429047, 0.6473214285714286031, 0.6517857142857143016, 0.6562500000000000000, 0.6607142857142856984, 0.6651785714285713969, 0.6696428571428570953, 0.6741071428571429047, 0.6785714285714286031, 0.6830357142857143016, 0.6875000000000000000, 0.6919642857142856984, 0.6964285714285713969, 0.7008928571428570953, 0.7053571428571429047, 0.7098214285714286031, 0.7142857142857143016, 0.7187500000000000000, 0.7232142857142856984, 0.7276785714285713969, 0.7321428571428570953, 0.7366071428571429047, 0.7410714285714286031, 0.7455357142857143016, 0.7500000000000000000, 0.7544642857142856984, 0.7589285714285713969, 0.7633928571428570953, 0.7678571428571429047, 0.7723214285714286031, 0.7767857142857143016, 0.7812500000000000000, 0.7857142857142856984, 0.7901785714285713969, 0.7946428571428570953, 0.7991071428571429047, 0.8035714285714286031, 0.8080357142857143016, 0.8125000000000000000, 0.8169642857142856984, 0.8214285714285713969, 0.8258928571428570953, 0.8303571428571429047, 0.8348214285714286031, 0.8392857142857143016, 0.8437500000000000000, 0.8482142857142856984, 0.8526785714285713969, 0.8571428571428570953, 0.8616071428571429047, 0.8660714285714286031, 0.8705357142857143016, 0.8750000000000000000, 0.8794642857142856984, 0.8839285714285713969, 0.8883928571428570953, 0.8928571428571429047, 0.8973214285714286031, 0.9017857142857143016, 0.9062500000000000000, 0.9107142857142856984, 0.9151785714285713969, 0.9196428571428570953, 0.9241071428571429047, 0.9285714285714286031, 0.9330357142857143016, 0.9375000000000000000, 0.9419642857142856984, 0.9464285714285713969, 0.9508928571428570953, 0.9553571428571429047, 0.9598214285714286031, 0.9642857142857143016, 0.9687500000000000000, 0.9732142857142856984, 0.9771335416943486285 ),
 .UNSPECIFIED. ) 
 GEOMETRIC_REPRESENTATION_ITEM ( )  RATIONAL_B_SPLINE_SURFACE ( (
 ( 1.000000000000000000, 0.9238795325112867385, 1.000000000000000000, 0.9238795325112867385, 1.000000000000000000, 0.9238795325112867385, 1.000000000000000000, 0.9238795325112867385, 1.000000000000000000, 0.9238795325112867385, 1.000000000000000000, 0.9238795325112867385, 1.000000000000000000, 0.9238795325112867385, 1.000000000000000000, 0.9238795325112867385, 1.000000000000000000, 0.9238795325112867385, 1.000000000000000000, 0.9238795325112867385, 1.000000000000000000, 0.9238795325112867385, 1.000000000000000000, 0.9238795325112867385, 1.000000000000000000, 0.9238795325112867385, 1.000000000000000000, 0.9238795325112867385, 1.000000000000000000, 0.9238795325112867385, 1.000000000000000000, 0.9238795325112867385, 1.000000000000000000, 0.9238795325112867385, 1.000000000000000000, 0.9238795325112867385, 1.000000000000000000, 0.9238795325112867385, 1.000000000000000000, 0.9238795325112867385, 1.000000000000000000, 0.9238795325112867385, 1.000000000000000000, 0.9238795325112867385, 1.000000000000000000, 0.9238795325112867385, 1.000000000000000000, 0.9238795325112867385, 1.000000000000000000, 0.9238795325112867385, 1.000000000000000000, 0.9238795325112867385, 1.000000000000000000, 0.9238795325112867385, 1.000000000000000000, 0.9238795325112867385, 1.000000000000000000, 0.9238795325112867385, 1.000000000000000000, 0.9238795325112867385, 1.000000000000000000, 0.9238795325112867385, 1.000000000000000000, 0.9238795325112867385, 1.000000000000000000, 0.9238795325112867385, 1.000000000000000000, 0.9238795325112867385, 1.000000000000000000, 0.9238795325112867385, 1.000000000000000000, 0.9238795325112867385, 1.000000000000000000, 0.9238795325112867385, 1.000000000000000000, 0.9238795325112867385, 1.000000000000000000, 0.9238795325112867385, 1.000000000000000000, 0.9238795325112867385, 1.000000000000000000, 0.9238795325112867385, 1.000000000000000000, 0.9238795325112867385, 1.000000000000000000, 0.9238795325112867385, 1.000000000000000000, 0.9238795325112867385, 1.000000000000000000, 0.9238795325112867385, 1.000000000000000000, 0.9238795325112867385, 1.000000000000000000, 0.9238795325112867385, 1.000000000000000000, 0.9238795325112867385, 1.000000000000000000, 0.9238795325112867385, 1.000000000000000000, 0.9238795325112867385, 1.000000000000000000, 0.9238795325112867385, 1.000000000000000000, 0.9238795325112867385, 1.000000000000000000, 0.9238795325112867385, 1.000000000000000000, 0.9238795325112867385, 1.000000000000000000, 0.9238795325112867385, 1.000000000000000000, 0.9238795325112867385, 1.000000000000000000, 0.9238795325112867385, 1.000000000000000000, 0.9238795325112867385, 1.000000000000000000, 0.9238795325112867385, 1.000000000000000000, 0.9238795325112867385, 1.000000000000000000, 0.9238795325112867385, 1.000000000000000000, 0.9238795325112867385, 1.000000000000000000, 0.9238795325112867385, 1.000000000000000000, 0.9238795325112867385, 1.000000000000000000, 0.9238795325112867385, 1.000000000000000000, 0.9238795325112867385, 1.000000000000000000, 0.9238795325112867385, 1.000000000000000000, 0.9238795325112867385, 1.000000000000000000, 0.9238795325112867385, 1.000000000000000000, 0.9238795325112867385, 1.000000000000000000, 0.9238795325112867385, 1.000000000000000000, 0.9238795325112867385, 1.000000000000000000, 0.9238795325112867385, 1.000000000000000000, 0.9238795325112867385, 1.000000000000000000, 0.9238795325112867385, 1.000000000000000000, 0.9238795325112867385, 1.000000000000000000, 0.9238795325112867385, 1.000000000000000000, 0.9238795325112867385, 1.000000000000000000, 0.9238795325112867385, 1.000000000000000000, 0.9238795325112867385, 1.000000000000000000, 0.9238795325112867385, 1.000000000000000000, 0.9238795325112867385, 1.000000000000000000, 0.9238795325112867385, 1.000000000000000000, 0.9238795325112867385, 1.000000000000000000, 0.9238795325112867385, 1.000000000000000000, 0.9238795325112867385, 1.000000000000000000, 0.9238795325112867385, 1.000000000000000000, 0.9238795325112867385, 1.000000000000000000, 0.9238795325112867385, 1.000000000000000000, 0.9238795325112867385, 1.000000000000000000, 0.9238795325112867385, 1.000000000000000000, 0.9238795325112867385, 1.000000000000000000, 0.9238795325112867385, 1.000000000000000000, 0.9238795325112867385, 1.000000000000000000, 0.9238795325112867385, 1.000000000000000000, 0.9238795325112867385, 1.000000000000000000, 0.9238795325112867385, 1.000000000000000000, 0.9238795325112867385, 1.000000000000000000, 0.9238795325112867385, 1.000000000000000000, 0.9238795325112867385, 1.000000000000000000, 0.9238795325112867385, 1.000000000000000000, 0.9238795325112867385, 1.000000000000000000, 0.9238795325112867385, 1.000000000000000000, 0.9238795325112867385, 1.000000000000000000, 0.9238795325112867385, 1.000000000000000000, 0.9238795325112867385, 1.000000000000000000, 0.9238795325112867385, 1.000000000000000000, 0.9238795325112867385, 1.000000000000000000, 0.9238795325112867385, 1.000000000000000000, 0.9238795325112867385, 1.000000000000000000, 0.9238795325112867385, 1.000000000000000000, 0.9238795325112867385, 1.000000000000000000, 0.9238795325112867385, 1.000000000000000000, 0.9238795325112867385, 1.000000000000000000, 0.9238795325112867385, 1.000000000000000000, 0.9238795325112867385, 1.000000000000000000, 0.9238795325112867385, 1.000000000000000000, 0.9238795325112867385, 1.000000000000000000, 0.9238795325112867385, 1.000000000000000000, 0.9238795325112867385, 1.000000000000000000, 0.9238795325112867385, 1.000000000000000000, 0.9238795325112867385, 1.000000000000000000, 0.9238795325112867385, 1.000000000000000000, 0.9238795325112867385, 1.000000000000000000, 0.9238795325112867385, 1.000000000000000000, 0.9238795325112867385, 1.000000000000000000, 0.9238795325112867385, 1.000000000000000000, 0.9238795325112867385, 1.000000000000000000, 0.9238795325112867385, 1.000000000000000000, 0.9238795325112867385, 1.000000000000000000, 0.9238795325112867385, 1.000000000000000000, 0.9238795325112867385, 1.000000000000000000, 0.9238795325112867385, 1.000000000000000000, 0.9238795325112867385, 1.000000000000000000, 0.9238795325112867385, 1.000000000000000000, 0.9238795325112867385, 1.000000000000000000, 0.9238795325112867385, 1.000000000000000000, 0.9238795325112867385, 1.000000000000000000, 0.9238795325112867385, 1.000000000000000000, 0.9238795325112867385, 1.000000000000000000, 0.9238795325112867385, 1.000000000000000000, 0.9238795325112867385, 1.000000000000000000, 0.9238795325112867385, 1.000000000000000000, 0.9238795325112867385, 1.000000000000000000, 0.9238795325112867385, 1.000000000000000000, 0.9238795325112867385, 1.000000000000000000, 0.9238795325112867385, 1.000000000000000000, 0.9238795325112867385, 1.000000000000000000, 0.9238795325112867385, 1.000000000000000000, 0.9238795325112867385, 1.000000000000000000, 0.9238795325112867385, 1.000000000000000000, 0.9238795325112867385, 1.000000000000000000, 0.9238795325112867385, 1.000000000000000000, 0.9238795325112867385, 1.000000000000000000, 0.9238795325112867385, 1.000000000000000000, 0.9238795325112867385, 1.000000000000000000, 0.9238795325112867385, 1.000000000000000000, 0.9238795325112867385, 1.000000000000000000, 0.9238795325112867385, 1.000000000000000000, 0.9238795325112867385, 1.000000000000000000, 0.9238795325112867385, 1.000000000000000000, 0.9238795325112867385, 1.000000000000000000, 0.9238795325112867385, 1.000000000000000000, 0.9238795325112867385, 1.000000000000000000, 0.9238795325112867385, 1.000000000000000000, 0.9238795325112867385, 1.000000000000000000, 0.9238795325112867385, 1.000000000000000000, 0.9238795325112867385, 1.000000000000000000, 0.9238795325112867385, 1.000000000000000000, 0.9238795325112867385, 1.000000000000000000, 0.9238795325112867385, 1.000000000000000000, 0.9238795325112867385, 1.000000000000000000, 0.9238795325112867385, 1.000000000000000000, 0.9238795325112867385, 1.000000000000000000, 0.9238795325112867385, 1.000000000000000000, 0.9238795325112867385, 1.000000000000000000, 0.9238795325112867385, 1.000000000000000000, 0.9238795325112867385, 1.000000000000000000, 0.9238795325112867385, 1.000000000000000000, 0.9238795325112867385, 1.000000000000000000, 0.9238795325112867385, 1.000000000000000000, 0.9238795325112867385, 1.000000000000000000, 0.9238795325112867385, 1.000000000000000000, 0.9238795325112867385, 1.000000000000000000, 0.9238795325112867385, 1.000000000000000000, 0.9238795325112867385, 1.000000000000000000, 0.9238795325112867385, 1.000000000000000000, 0.9238795325112867385, 1.000000000000000000, 0.9238795325112867385, 1.000000000000000000, 0.9238795325112867385, 1.000000000000000000, 0.9238795325112867385, 1.000000000000000000, 0.9238795325112867385, 1.000000000000000000, 0.9238795325112867385, 1.000000000000000000, 0.9238795325112867385, 1.000000000000000000, 0.9238795325112867385, 1.000000000000000000, 0.9238795325112867385, 1.000000000000000000, 0.9238795325112867385, 1.000000000000000000, 0.9238795325112867385, 1.000000000000000000, 0.9238795325112867385, 1.000000000000000000, 0.9238795325112867385, 1.000000000000000000, 0.9238795325112867385, 1.000000000000000000, 0.9238795325112867385, 1.000000000000000000, 0.9238795325112867385, 1.000000000000000000, 0.9238795325112867385, 1.000000000000000000, 0.9238795325112867385, 1.000000000000000000, 0.9238795325112867385, 1.000000000000000000, 0.9238795325112867385, 1.000000000000000000, 0.9238795325112867385, 1.000000000000000000, 0.9238795325112867385, 1.000000000000000000, 0.9238795325112867385, 1.000000000000000000, 0.9238795325112867385, 1.000000000000000000, 0.9238795325112867385, 1.000000000000000000, 0.9238795325112867385, 1.000000000000000000, 0.9238795325112867385, 1.000000000000000000, 0.9238795325112867385, 1.000000000000000000, 0.9238795325112867385, 1.000000000000000000, 0.9238795325112867385, 1.000000000000000000, 0.9238795325112867385, 1.000000000000000000, 0.9331728261800869006, 0.9836825870399050764),
 ( 1.000000000000000000, 0.9238795325112867385, 1.000000000000000000, 0.9238795325112867385, 1.000000000000000000, 0.9238795325112867385, 1.000000000000000000, 0.9238795325112867385, 1.000000000000000000, 0.9238795325112867385, 1.000000000000000000, 0.9238795325112867385, 1.000000000000000000, 0.9238795325112867385, 1.000000000000000000, 0.9238795325112867385, 1.000000000000000000, 0.9238795325112867385, 1.000000000000000000, 0.9238795325112867385, 1.000000000000000000, 0.9238795325112867385, 1.000000000000000000, 0.9238795325112867385, 1.000000000000000000, 0.9238795325112867385, 1.000000000000000000, 0.9238795325112867385, 1.000000000000000000, 0.9238795325112867385, 1.000000000000000000, 0.9238795325112867385, 1.000000000000000000, 0.9238795325112867385, 1.000000000000000000, 0.9238795325112867385, 1.000000000000000000, 0.9238795325112867385, 1.000000000000000000, 0.9238795325112867385, 1.000000000000000000, 0.9238795325112867385, 1.000000000000000000, 0.9238795325112867385, 1.000000000000000000, 0.9238795325112867385, 1.000000000000000000, 0.9238795325112867385, 1.000000000000000000, 0.9238795325112867385, 1.000000000000000000, 0.9238795325112867385, 1.000000000000000000, 0.9238795325112867385, 1.000000000000000000, 0.9238795325112867385, 1.000000000000000000, 0.9238795325112867385, 1.000000000000000000, 0.9238795325112867385, 1.000000000000000000, 0.9238795325112867385, 1.000000000000000000, 0.9238795325112867385, 1.000000000000000000, 0.9238795325112867385, 1.000000000000000000, 0.9238795325112867385, 1.000000000000000000, 0.9238795325112867385, 1.000000000000000000, 0.9238795325112867385, 1.000000000000000000, 0.9238795325112867385, 1.000000000000000000, 0.9238795325112867385, 1.000000000000000000, 0.9238795325112867385, 1.000000000000000000, 0.9238795325112867385, 1.000000000000000000, 0.9238795325112867385, 1.000000000000000000, 0.9238795325112867385, 1.000000000000000000, 0.9238795325112867385, 1.000000000000000000, 0.9238795325112867385, 1.000000000000000000, 0.9238795325112867385, 1.000000000000000000, 0.9238795325112867385, 1.000000000000000000, 0.9238795325112867385, 1.000000000000000000, 0.9238795325112867385, 1.000000000000000000, 0.9238795325112867385, 1.000000000000000000, 0.9238795325112867385, 1.000000000000000000, 0.9238795325112867385, 1.000000000000000000, 0.9238795325112867385, 1.000000000000000000, 0.9238795325112867385, 1.000000000000000000, 0.9238795325112867385, 1.000000000000000000, 0.9238795325112867385, 1.000000000000000000, 0.9238795325112867385, 1.000000000000000000, 0.9238795325112867385, 1.000000000000000000, 0.9238795325112867385, 1.000000000000000000, 0.9238795325112867385, 1.000000000000000000, 0.9238795325112867385, 1.000000000000000000, 0.9238795325112867385, 1.000000000000000000, 0.9238795325112867385, 1.000000000000000000, 0.9238795325112867385, 1.000000000000000000, 0.9238795325112867385, 1.000000000000000000, 0.9238795325112867385, 1.000000000000000000, 0.9238795325112867385, 1.000000000000000000, 0.9238795325112867385, 1.000000000000000000, 0.9238795325112867385, 1.000000000000000000, 0.9238795325112867385, 1.000000000000000000, 0.9238795325112867385, 1.000000000000000000, 0.9238795325112867385, 1.000000000000000000, 0.9238795325112867385, 1.000000000000000000, 0.9238795325112867385, 1.000000000000000000, 0.9238795325112867385, 1.000000000000000000, 0.9238795325112867385, 1.000000000000000000, 0.9238795325112867385, 1.000000000000000000, 0.9238795325112867385, 1.000000000000000000, 0.9238795325112867385, 1.000000000000000000, 0.9238795325112867385, 1.000000000000000000, 0.9238795325112867385, 1.000000000000000000, 0.9238795325112867385, 1.000000000000000000, 0.9238795325112867385, 1.000000000000000000, 0.9238795325112867385, 1.000000000000000000, 0.9238795325112867385, 1.000000000000000000, 0.9238795325112867385, 1.000000000000000000, 0.9238795325112867385, 1.000000000000000000, 0.9238795325112867385, 1.000000000000000000, 0.9238795325112867385, 1.000000000000000000, 0.9238795325112867385, 1.000000000000000000, 0.9238795325112867385, 1.000000000000000000, 0.9238795325112867385, 1.000000000000000000, 0.9238795325112867385, 1.000000000000000000, 0.9238795325112867385, 1.000000000000000000, 0.9238795325112867385, 1.000000000000000000, 0.9238795325112867385, 1.000000000000000000, 0.9238795325112867385, 1.000000000000000000, 0.9238795325112867385, 1.000000000000000000, 0.9238795325112867385, 1.000000000000000000, 0.9238795325112867385, 1.000000000000000000, 0.9238795325112867385, 1.000000000000000000, 0.9238795325112867385, 1.000000000000000000, 0.9238795325112867385, 1.000000000000000000, 0.9238795325112867385, 1.000000000000000000, 0.9238795325112867385, 1.000000000000000000, 0.9238795325112867385, 1.000000000000000000, 0.9238795325112867385, 1.000000000000000000, 0.9238795325112867385, 1.000000000000000000, 0.9238795325112867385, 1.000000000000000000, 0.9238795325112867385, 1.000000000000000000, 0.9238795325112867385, 1.000000000000000000, 0.9238795325112867385, 1.000000000000000000, 0.9238795325112867385, 1.000000000000000000, 0.9238795325112867385, 1.000000000000000000, 0.9238795325112867385, 1.000000000000000000, 0.9238795325112867385, 1.000000000000000000, 0.9238795325112867385, 1.000000000000000000, 0.9238795325112867385, 1.000000000000000000, 0.9238795325112867385, 1.000000000000000000, 0.9238795325112867385, 1.000000000000000000, 0.9238795325112867385, 1.000000000000000000, 0.9238795325112867385, 1.000000000000000000, 0.9238795325112867385, 1.000000000000000000, 0.9238795325112867385, 1.000000000000000000, 0.9238795325112867385, 1.000000000000000000, 0.9238795325112867385, 1.000000000000000000, 0.9238795325112867385, 1.000000000000000000, 0.9238795325112867385, 1.000000000000000000, 0.9238795325112867385, 1.000000000000000000, 0.9238795325112867385, 1.000000000000000000, 0.9238795325112867385, 1.000000000000000000, 0.9238795325112867385, 1.000000000000000000, 0.9238795325112867385, 1.000000000000000000, 0.9238795325112867385, 1.000000000000000000, 0.9238795325112867385, 1.000000000000000000, 0.9238795325112867385, 1.000000000000000000, 0.9238795325112867385, 1.000000000000000000, 0.9238795325112867385, 1.000000000000000000, 0.9238795325112867385, 1.000000000000000000, 0.9238795325112867385, 1.000000000000000000, 0.9238795325112867385, 1.000000000000000000, 0.9238795325112867385, 1.000000000000000000, 0.9238795325112867385, 1.000000000000000000, 0.9238795325112867385, 1.000000000000000000, 0.9238795325112867385, 1.000000000000000000, 0.9238795325112867385, 1.000000000000000000, 0.9238795325112867385, 1.000000000000000000, 0.9238795325112867385, 1.000000000000000000, 0.9238795325112867385, 1.000000000000000000, 0.9238795325112867385, 1.000000000000000000, 0.9238795325112867385, 1.000000000000000000, 0.9238795325112867385, 1.000000000000000000, 0.9238795325112867385, 1.000000000000000000, 0.9238795325112867385, 1.000000000000000000, 0.9238795325112867385, 1.000000000000000000, 0.9238795325112867385, 1.000000000000000000, 0.9238795325112867385, 1.000000000000000000, 0.9238795325112867385, 1.000000000000000000, 0.9238795325112867385, 1.000000000000000000, 0.9238795325112867385, 1.000000000000000000, 0.9238795325112867385, 1.000000000000000000, 0.9238795325112867385, 1.000000000000000000, 0.9238795325112867385, 1.000000000000000000, 0.9238795325112867385, 1.000000000000000000, 0.9238795325112867385, 1.000000000000000000, 0.9238795325112867385, 1.000000000000000000, 0.9238795325112867385, 1.000000000000000000, 0.9238795325112867385, 1.000000000000000000, 0.9238795325112867385, 1.000000000000000000, 0.9238795325112867385, 1.000000000000000000, 0.9238795325112867385, 1.000000000000000000, 0.9238795325112867385, 1.000000000000000000, 0.9238795325112867385, 1.000000000000000000, 0.9238795325112867385, 1.000000000000000000, 0.9238795325112867385, 1.000000000000000000, 0.9238795325112867385, 1.000000000000000000, 0.9238795325112867385, 1.000000000000000000, 0.9238795325112867385, 1.000000000000000000, 0.9238795325112867385, 1.000000000000000000, 0.9238795325112867385, 1.000000000000000000, 0.9238795325112867385, 1.000000000000000000, 0.9238795325112867385, 1.000000000000000000, 0.9238795325112867385, 1.000000000000000000, 0.9238795325112867385, 1.000000000000000000, 0.9238795325112867385, 1.000000000000000000, 0.9238795325112867385, 1.000000000000000000, 0.9238795325112867385, 1.000000000000000000, 0.9238795325112867385, 1.000000000000000000, 0.9238795325112867385, 1.000000000000000000, 0.9238795325112867385, 1.000000000000000000, 0.9238795325112867385, 1.000000000000000000, 0.9238795325112867385, 1.000000000000000000, 0.9238795325112867385, 1.000000000000000000, 0.9238795325112867385, 1.000000000000000000, 0.9238795325112867385, 1.000000000000000000, 0.9238795325112867385, 1.000000000000000000, 0.9238795325112867385, 1.000000000000000000, 0.9238795325112867385, 1.000000000000000000, 0.9238795325112867385, 1.000000000000000000, 0.9238795325112867385, 1.000000000000000000, 0.9238795325112867385, 1.000000000000000000, 0.9238795325112867385, 1.000000000000000000, 0.9238795325112867385, 1.000000000000000000, 0.9238795325112867385, 1.000000000000000000, 0.9238795325112867385, 1.000000000000000000, 0.9238795325112867385, 1.000000000000000000, 0.9238795325112867385, 1.000000000000000000, 0.9238795325112867385, 1.000000000000000000, 0.9238795325112867385, 1.000000000000000000, 0.9238795325112867385, 1.000000000000000000, 0.9238795325112867385, 1.000000000000000000, 0.9238795325112867385, 1.000000000000000000, 0.9238795325112867385, 1.000000000000000000, 0.9238795325112867385, 1.000000000000000000, 0.9238795325112867385, 1.000000000000000000, 0.9238795325112867385, 1.000000000000000000, 0.9238795325112867385, 1.000000000000000000, 0.9238795325112867385, 1.000000000000000000, 0.9238795325112867385, 1.000000000000000000, 0.9331728261800869006, 0.9836825870399050764) ) ) 
 REPRESENTATION_ITEM ( '' )  SURFACE ( )  );
#16472 = CARTESIAN_POINT ( 'NONE',  ( 0.4593754077519624501, -0.04467882043364388572, 0.4343923118385376592 ) ) ;
#16473 = CARTESIAN_POINT ( 'NONE',  ( 0.1167790944451423257, 0.6013888888130223265, -0.2819296736111110424 ) ) ;
#16474 = CARTESIAN_POINT ( 'NONE',  ( 0.1167790944451424368, 3.828555555631421470, 0.2819296736111110424 ) ) ;
#16475 = CARTESIAN_POINT ( 'NONE',  ( 0.3613381517857143232, 0.2937499999024575370, 0.1174058825155742114 ) ) ;
#16476 = CARTESIAN_POINT ( 'NONE',  ( -0.2819296736111110424, 4.536888888964754507, 0.1167790944451424923 ) ) ;
#16477 = CARTESIAN_POINT ( 'NONE',  ( 0.3084175934503982641, -2.427762526784286478E-18, -0.1882653658700420007 ) ) ;
#16478 = EDGE_CURVE ( 'NONE', #8144, #22410, #19950, .T. ) ;
#16479 = CARTESIAN_POINT ( 'NONE',  ( -0.2206173157302028232, 4.599388888888888083, -0.2206173157302028232 ) ) ;
#16480 = EDGE_CURVE ( 'NONE', #15406, #6253, #21531, .T. ) ;
#16481 = ORIENTED_EDGE ( 'NONE', *, *, #12026, .T. ) ;
#16482 = EDGE_CURVE ( 'NONE', #23140, #280, #15922, .T. ) ;
#16483 = CARTESIAN_POINT ( 'NONE',  ( 0.4000000000000000222, 0.3999999999999999112, 0.000000000000000000 ) ) ;
#16484 = CARTESIAN_POINT ( 'NONE',  ( -1.910449006669871087E-17, 3.710500000151732092, -0.3119999999999999996 ) ) ;
#16485 = CARTESIAN_POINT ( 'NONE',  ( 0.3110561587738748246, 4.195609504020111125, 0.03575875776001819634 ) ) ;
#16486 = ADVANCED_FACE ( 'NONE', ( #10332 ), #5947, .F. ) ;
#16487 = CARTESIAN_POINT ( 'NONE',  ( -5.731347020009612645E-17, 0.5041666666666663188, 0.3119999999999999996 ) ) ;
#16488 = CARTESIAN_POINT ( 'NONE',  ( 0.1236067977499789861, 0.1999999999999999278, -0.3804226065180614236 ) ) ;
#16489 = CARTESIAN_POINT ( 'NONE',  ( -0.2819296736111110979, 4.630638888964754507, 0.000000000000000000 ) ) ;
#16490 = SECURITY_CLASSIFICATION_LEVEL ( 'unclassified' ) ;
#16491 = VECTOR ( 'NONE', #21227, 39.37007874015748143 ) ;
#16492 = CARTESIAN_POINT ( 'NONE',  ( -0.1292346314604068958, 4.762583333333332725, -0.3119999999999987228 ) ) ;
#16493 = CARTESIAN_POINT ( 'NONE',  ( -0.001863919267180048824, -0.003009961218012348859, 2.816660016782450704 ) ) ;
#16494 = CARTESIAN_POINT ( 'NONE',  ( -0.1993543840281266633, 0.2368055554796889006, -0.1993543840281266910 ) ) ;
#16495 = ORIENTED_EDGE ( 'NONE', *, *, #4185, .F. ) ;
#16496 = CARTESIAN_POINT ( 'NONE',  ( -0.2819296736111110979, 0.1326388888130222710, -3.452642723725051716E-17 ) ) ;
#16497 = CARTESIAN_POINT ( 'NONE',  ( -0.2549684922721914271, 5.198137420699272759, -0.1298580064688831803 ) ) ;
#16498 = CARTESIAN_POINT ( 'NONE',  ( 0.3236067977499789694, 0.03571428571428568455, 0.2351141009169893659 ) ) ;
#16499 = CARTESIAN_POINT ( 'NONE',  ( -0.1306872919485615459, -0.3155070326520293400, -0.09395833333333311610 ) ) ;
#16500 = CARTESIAN_POINT ( 'NONE',  ( 0.3125000000000000000, -5.740531871003217465E-17, 0.4216666666666709085 ) ) ;
#16501 = EDGE_CURVE ( 'NONE', #17619, #6124, #23464, .T. ) ;
#16502 = CARTESIAN_POINT ( 'NONE',  ( -0.2685268980859171206, 3.886276269974404229, -0.1597531070831219036 ) ) ;
#16503 = CARTESIAN_POINT ( 'NONE',  ( -0.2819296736111110979, 0.06666666659080003332, 0.1167790944451422425 ) ) ;
#16504 = CARTESIAN_POINT ( 'NONE',  ( 0.1167790944451422702, 4.460500000075867000, -0.2819296736111110424 ) ) ;
#16505 = CARTESIAN_POINT ( 'NONE',  ( 0.1236067977499789861, 0.1910714283763437493, -0.3804226065180614236 ) ) ;
#16506 = CARTESIAN_POINT ( 'NONE',  ( -0.06335377612981435425, 0.1570980611782421266, 0.4000000000000000777 ) ) ;
#16507 = CARTESIAN_POINT ( 'NONE',  ( 0.2819296736111110424, 5.009111111186976828, -0.1167790944451423396 ) ) ;
#16508 = CARTESIAN_POINT ( 'NONE',  ( 0.4450000000000002842, 0.000000000000000000, -2.540999999999999925 ) ) ;
#16509 = CARTESIAN_POINT ( 'NONE',  ( 0.3027533619087663386, 3.750030080416155265, 0.07586331988550912286 ) ) ;
#16510 = CARTESIAN_POINT ( 'NONE',  ( -0.6396424860381280109, 0.000000000000000000, -0.01143517789850382292 ) ) ;
#16511 = CARTESIAN_POINT ( 'NONE',  ( -0.1590601067977006067, 0.4494324818882923789, 0.07654795713853398964 ) ) ;
#16512 = CARTESIAN_POINT ( 'NONE',  ( 0.3119999999999999996, 4.359805555707287894, 0.1292346314604056190 ) ) ;
#16513 = CIRCLE ( 'NONE', #8712, 0.01874999999999999584 ) ;
#16514 = CARTESIAN_POINT ( 'NONE',  ( -0.1993543840281266355, 4.540361111186976828, 0.1993543840281267465 ) ) ;
#16515 = CARTESIAN_POINT ( 'NONE',  ( -0.2819296736111110424, 3.738277777853643347, -0.1167790944451423119 ) ) ;
#16516 = EDGE_CURVE ( 'NONE', #8318, #11791, #2056, .T. ) ;
#16517 = VERTEX_POINT ( 'NONE', #23226 ) ;
#16518 = ORIENTED_EDGE ( 'NONE', *, *, #6308, .T. ) ;
#16519 = DATE_AND_TIME ( #8828, #7990 ) ;
#16520 = CARTESIAN_POINT ( 'NONE',  ( -0.2460300421372414448, -0.1745426587114260741, 0.4128571377276832877 ) ) ;
#16521 = LINE ( 'NONE', #1401, #5656 ) ;
#16522 = DIRECTION ( 'NONE',  ( 0.000000000000000000, 0.000000000000000000, 1.000000000000000000 ) ) ;
#16523 = VERTEX_POINT ( 'NONE', #21775 ) ;
#16524 = CARTESIAN_POINT ( 'NONE',  ( -0.2206173157302028787, 0.3236111109593782231, 0.2206173157302027954 ) ) ;
#16525 = CARTESIAN_POINT ( 'NONE',  ( 0.000000000000000000, 3.700000000000000622, 0.000000000000000000 ) ) ;
#16526 = CARTESIAN_POINT ( 'NONE',  ( -0.1852720301558682114, 3.732674766298908597, 0.2552238848127614257 ) ) ;
#16527 = VECTOR ( 'NONE', #20936, 39.37007874015748143 ) ;
#16528 = DIRECTION ( 'NONE',  ( 0.7071067811865435759, 0.7071067811865514585, 0.000000000000000000 ) ) ;
#16529 = DIRECTION ( 'NONE',  ( 1.000000000000000000, 0.000000000000000000, 0.000000000000000000 ) ) ;
#16530 = ORIENTED_EDGE ( 'NONE', *, *, #20114, .T. ) ;
#16531 = CARTESIAN_POINT ( 'NONE',  ( 0.2233192592356400275, 0.02232142847388617762, -0.3073725909049499494 ) ) ;
#16532 = VERTEX_POINT ( 'NONE', #4819 ) ;
#16533 = CARTESIAN_POINT ( 'NONE',  ( 0.2882303765580553900, 5.089197615778912720, -0.1187411923064577435 ) ) ;
#16534 = CARTESIAN_POINT ( 'NONE',  ( -0.1954553509668046640, 0.1954553509668046918, 0.2480555555555586933 ) ) ;
#16535 = CARTESIAN_POINT ( 'NONE',  ( -1.726321361862525858E-17, 4.172305555631420582, -0.2819296736111110979 ) ) ;
#16536 = CARTESIAN_POINT ( 'NONE',  ( -0.2819296736111110979, 5.182722222298087544, -0.1167790944451422980 ) ) ;
#16537 = LINE ( 'NONE', #20072, #11814 ) ;
#16538 = CARTESIAN_POINT ( 'NONE',  ( -0.05810125945330829600, 4.236650434042510405, 0.3066015745271455373 ) ) ;
#16539 = AXIS2_PLACEMENT_3D ( 'NONE', #13316, #370, #7812 ) ;
#16540 = CARTESIAN_POINT ( 'NONE',  ( -1.910449006669871087E-17, 4.092444444444444329, -0.3119999999999999996 ) ) ;
#16541 = CARTESIAN_POINT ( 'NONE',  ( -0.2206173157302027676, 4.898000000151732536, 0.2206173157302028787 ) ) ;
#16542 = CARTESIAN_POINT ( 'NONE',  ( -0.2819296736111110979, 5.196611111186976828, -0.1167790944451422980 ) ) ;
#16543 = DIRECTION ( 'NONE',  ( 0.000000000000000000, 0.000000000000000000, -1.000000000000000000 ) ) ;
#16544 = CIRCLE ( 'NONE', #6420, 0.01874999999999997155 ) ;
#16545 = DIRECTION ( 'NONE',  ( -0.5000000000000003331, 0.8660254037844383745, 0.000000000000000000 ) ) ;
#16546 = ORIENTED_EDGE ( 'NONE', *, *, #16243, .T. ) ;
#16547 = CARTESIAN_POINT ( 'NONE',  ( 0.1306872919485614071, -0.3155070326520293955, 0.2497916666666700480 ) ) ;
#16548 = CARTESIAN_POINT ( 'NONE',  ( 5.178964085587577574E-17, 5.088972222298087544, 0.2819296736111110979 ) ) ;
#16549 =( GEOMETRIC_REPRESENTATION_CONTEXT ( 3 ) GLOBAL_UNCERTAINTY_ASSIGNED_CONTEXT ( ( #13649 ) ) GLOBAL_UNIT_ASSIGNED_CONTEXT ( ( #18664, #20974, #10136 ) ) REPRESENTATION_CONTEXT ( 'NONE', 'WORKASPACE' ) );
#16550 = CARTESIAN_POINT ( 'NONE',  ( 0.4000000000000000222, 0.04285714285714282978, 0.000000000000000000 ) ) ;
#16551 = PRODUCT_DEFINITION_SHAPE ( 'NONE', 'NONE',  #24133 ) ;
#16552 = CARTESIAN_POINT ( 'NONE',  ( -0.3613381517857144343, 0.3901785713310290116, 0.1174058825155740171 ) ) ;
#16553 = CARTESIAN_POINT ( 'NONE',  ( 0.1167790944451423535, 0.3722222221463555858, 0.2819296736111110979 ) ) ;
#16554 = CARTESIAN_POINT ( 'NONE',  ( -0.2764156081756484196, 1.692557448933383907E-17, 0.2619444444444476994 ) ) ;
#16555 = CARTESIAN_POINT ( 'NONE',  ( 0.2819296736111110979, 4.950083333409199149, -3.452642723725051716E-17 ) ) ;
#16556 = CARTESIAN_POINT ( 'NONE',  ( 0.3052904481388406532, 4.472585030868217792, 0.06436050040701235542 ) ) ;
#16557 = VECTOR ( 'NONE', #2058, 39.37007874015748143 ) ;
#16558 = ORIENTED_EDGE ( 'NONE', *, *, #20607, .F. ) ;
#16559 = CARTESIAN_POINT ( 'NONE',  ( -0.1993543840281266910, 4.790361111186976828, -0.1993543840281266910 ) ) ;
#16560 = CARTESIAN_POINT ( 'NONE',  ( -0.1914713219046094150, 4.160640935953036745, -0.2497021521199800087 ) ) ;
#16561 = CARTESIAN_POINT ( 'NONE',  ( -0.1166234456863465552, 3.066692553488282957, 2.711183489075826181 ) ) ;
#16562 = CARTESIAN_POINT ( 'NONE',  ( 2.986000000000000210, 2.740000000000000213, -0.07500000000000014988 ) ) ;
#16563 = CARTESIAN_POINT ( 'NONE',  ( 1.938418520877619899, 2.405295409249399441, -1.890758069268034136 ) ) ;
#16564 = CARTESIAN_POINT ( 'NONE',  ( -0.3119999999999999996, 4.769527777777776478, -0.1292346314604056468 ) ) ;
#16565 = CARTESIAN_POINT ( 'NONE',  ( 0.2819296736111111534, 4.043833333409200037, 0.1167790944451422563 ) ) ;
#16566 = DIRECTION ( 'NONE',  ( 0.000000000000000000, -0.9961946980917454342, 0.08715574274765845730 ) ) ;
#16567 = CARTESIAN_POINT ( 'NONE',  ( 0.1864095630950551863, 4.021751787035609205, 0.2501916434414996893 ) ) ;
#16568 = CARTESIAN_POINT ( 'NONE',  ( 0.008438385721237055825, 0.5369265497013592237, 0.04763613967037114844 ) ) ;
#16569 = LOCAL_TIME ( 21, 9, 13.00000000000000000, #14205 ) ;
#16570 = ORIENTED_EDGE ( 'NONE', *, *, #2572, .T. ) ;
#16571 = VERTEX_POINT ( 'NONE', #19828 ) ;
#16572 = CARTESIAN_POINT ( 'NONE',  ( 0.2209708691207961095, -0.2209708691207961651, 0.1369444444444465059 ) ) ;
#16573 = CARTESIAN_POINT ( 'NONE',  ( -0.2156887100776810617, -0.4167379425407622962, 0.4181572966874574915 ) ) ;
#16574 = AXIS2_PLACEMENT_3D ( 'NONE', #22009, #5179, #16652 ) ;
#16575 = CARTESIAN_POINT ( 'NONE',  ( 1.573500000000000343, 0.000000000000000000, -0.3524999999999999800 ) ) ;
#16576 = CARTESIAN_POINT ( 'NONE',  ( 0.1954553509668046640, -0.1954553509668047195, 0.1647222222222247123 ) ) ;
#16577 = CARTESIAN_POINT ( 'NONE',  ( 0.3125000000000000000, -5.740531871003217465E-17, 0.1508333333333358728 ) ) ;
#16578 = CARTESIAN_POINT ( 'NONE',  ( -0.2726262432888192366, 4.442052030412000363, -0.1571209434472312649 ) ) ;
#16579 = CARTESIAN_POINT ( 'NONE',  ( 1.573500000000000343, 0.5250000000000000222, -0.3524999999999999800 ) ) ;
#16580 = CARTESIAN_POINT ( 'NONE',  ( -0.1116596296178199582, 0.3901785713310289561, -0.3436530038418508792 ) ) ;
#16581 = CARTESIAN_POINT ( 'NONE',  ( -5.178964085587577574E-17, 0.1881944443685778512, 0.2819296736111110979 ) ) ;
#16582 = CARTESIAN_POINT ( 'NONE',  ( 0.4802534614900670906, -0.2139706815658275474, 0.05347077774226097896 ) ) ;
#16583 = CARTESIAN_POINT ( 'NONE',  ( 0.3119999999999998885, 0.5701388888888886397, 0.1292346314604058410 ) ) ;
#16584 = EDGE_CURVE ( 'NONE', #6836, #17018, #5061, .T. ) ;
#16585 = CARTESIAN_POINT ( 'NONE',  ( -0.05588159907449195135, 0.5841765427403826649, -0.7479453483804153757 ) ) ;
#16586 = CARTESIAN_POINT ( 'NONE',  ( -0.2764156081756484196, 1.692557448933383907E-17, -0.01583333333333230425 ) ) ;
#16587 = ORIENTED_EDGE ( 'NONE', *, *, #13344, .F. ) ;
#16588 = VERTEX_POINT ( 'NONE', #18122 ) ;
#16589 = CARTESIAN_POINT ( 'NONE',  ( -0.3103325563594151459, 5.105850683298335468, 0.01916239243782727822 ) ) ;
#16590 = CARTESIAN_POINT ( 'NONE',  ( 0.008081987039816235924, 1.999640111863030256, -3.301832351584418568 ) ) ;
#16591 = CARTESIAN_POINT ( 'NONE',  ( -0.2206173157302027954, -0.01666666666666700297, -0.2206173157302028232 ) ) ;
#16592 = CARTESIAN_POINT ( 'NONE',  ( -0.1167790944451423257, 3.745222222298088433, -0.2819296736111110424 ) ) ;
#16593 = CARTESIAN_POINT ( 'NONE',  ( 0.2233192592356399997, 0.1651785713310290615, -0.3073725909049500049 ) ) ;
#16594 = VECTOR ( 'NONE', #3843, 39.37007874015748854 ) ;
#16595 = ADVANCED_FACE ( 'NONE', ( #8848 ), #1053, .T. ) ;
#16596 = CARTESIAN_POINT ( 'NONE',  ( 0.1167790944451424368, 4.384111111186976828, 0.2819296736111110424 ) ) ;
#16597 = CARTESIAN_POINT ( 'NONE',  ( 0.2206173157302027954, 4.974388888888888083, -0.2206173157302028232 ) ) ;
#16598 = FACE_OUTER_BOUND ( 'NONE', #21155, .T. ) ;
#16599 = ORIENTED_EDGE ( 'NONE', *, *, #20194, .T. ) ;
#16600 = CARTESIAN_POINT ( 'NONE',  ( 0.2595622703492775907, 4.358042815605328357, 0.1731226536284558581 ) ) ;
#16601 = CARTESIAN_POINT ( 'NONE',  ( -0.2819296736111110979, 4.852861111186976828, 0.000000000000000000 ) ) ;
#16602 = CC_DESIGN_APPROVAL ( #5231, ( #4895 ) ) ;
#16603 = FACE_OUTER_BOUND ( 'NONE', #12380, .T. ) ;
#16604 =( LENGTH_UNIT ( ) NAMED_UNIT ( * ) SI_UNIT ( $, .METRE. ) );
#16605 = CARTESIAN_POINT ( 'NONE',  ( 5.731347020009612645E-17, 5.009111111111110404, 0.3119999999999999996 ) ) ;
#16606 = CARTESIAN_POINT ( 'NONE',  ( 0.1167790944451422702, 4.779944444520308977, -0.2819296736111110979 ) ) ;
#16607 = DATE_TIME_ROLE ( 'classification_date' ) ;
#16608 = CARTESIAN_POINT ( 'NONE',  ( -0.4805453593044316518, 0.2624503992731411772, 0.04271845132551600754 ) ) ;
#16609 =( BOUNDED_CURVE ( )  B_SPLINE_CURVE ( 2, ( #11562, #11679, #18989, #2408, #2288, #9848, #22645, #5697, #327 ),
 .UNSPECIFIED., .F., .F. ) 
 B_SPLINE_CURVE_WITH_KNOTS ( ( 3, 2, 2, 2, 3 ),
 ( 0.8482142857142856984, 0.8526785714285713969, 0.8571428571428569843, 0.8616071428571427937, 0.8660714285714284921 ),
 .UNSPECIFIED. ) 
 CURVE ( )  GEOMETRIC_REPRESENTATION_ITEM ( )  RATIONAL_B_SPLINE_CURVE ( ( 1.000000000000000000, 0.9238795325112867385, 1.000000000000000000, 0.9238795325112867385, 1.000000000000000000, 0.9238795325112867385, 1.000000000000000000, 0.9238795325112886259, 0.9999999999999981126 ) ) 
 REPRESENTATION_ITEM ( '' )  );
#16610 = CARTESIAN_POINT ( 'NONE',  ( 0.1167790944451423535, 0.4277777777019111105, 0.2819296736111110424 ) ) ;
#16611 = ADVANCED_FACE ( 'NONE', ( #12050 ), #2873, .T. ) ;
#16612 = ORIENTED_EDGE ( 'NONE', *, *, #22778, .T. ) ;
#16613 = VERTEX_POINT ( 'NONE', #17759 ) ;
#16614 = CARTESIAN_POINT ( 'NONE',  ( 0.2819296736111110979, 0.1604166665908000333, 0.000000000000000000 ) ) ;
#16615 = DIRECTION ( 'NONE',  ( 0.000000000000000000, 0.000000000000000000, 1.000000000000000000 ) ) ;
#16616 = CARTESIAN_POINT ( 'NONE',  ( -0.2778555843174162487, 5.199876218914782910, -0.06507818477629406795 ) ) ;
#16617 = CARTESIAN_POINT ( 'NONE',  ( 0.3613381517857143232, 0.4187499999024575370, 0.1174058825155742114 ) ) ;
#16618 = CARTESIAN_POINT ( 'NONE',  ( 0.000000000000000000, 0.3155070326520292845, -0.06270833333333286630 ) ) ;
#16619 = CARTESIAN_POINT ( 'NONE',  ( 0.4687500000000002776, 0.2598076211353318454, 0.3779506566538942125 ) ) ;
#16620 = CARTESIAN_POINT ( 'NONE',  ( -0.2567736115681932274, 3.885679132990351281, -0.1772326254732079776 ) ) ;
#16621 = CARTESIAN_POINT ( 'NONE',  ( 0.9244709581221690620, 2.291712385858714285, -1.333428253224823168 ) ) ;
#16622 = CARTESIAN_POINT ( 'NONE',  ( -1.726321361862525858E-17, 4.463972222298087544, -0.2819296736111110979 ) ) ;
#16623 = ORIENTED_EDGE ( 'NONE', *, *, #19414, .F. ) ;
#16624 = CARTESIAN_POINT ( 'NONE',  ( 0.3999999999999999667, 0.03749999980491521001, -0.1299678784931625475 ) ) ;
#16625 = CARTESIAN_POINT ( 'NONE',  ( 0.1562950836073939143, 4.539213769334139670, -0.2717496176494637594 ) ) ;
#16626 = ADVANCED_FACE ( 'NONE', ( #10212 ), #6535, .T. ) ;
#16627 = CARTESIAN_POINT ( 'NONE',  ( -1.726321361862525858E-17, 5.075083333409198261, -0.2819296736111110979 ) ) ;
#16628 = CARTESIAN_POINT ( 'NONE',  ( 0.1167790944451424506, 4.370222222298088433, 0.2819296736111110424 ) ) ;
#16629 = CARTESIAN_POINT ( 'NONE',  ( 0.2151400685697778814, 3.744996934445992132, 0.2277764084372883857 ) ) ;
#16630 = CARTESIAN_POINT ( 'NONE',  ( 3.820898013339742174E-17, 5.384999999999999787, 0.3119999999999999996 ) ) ;
#16631 = AXIS2_PLACEMENT_3D ( 'NONE', #2344, #9782, #13215 ) ;
#16632 = CARTESIAN_POINT ( 'NONE',  ( 0.000000000000000000, 0.000000000000000000, -0.05999999999999999084 ) ) ;
#16633 = CARTESIAN_POINT ( 'NONE',  ( 0.1292346314604058410, 4.130638889040620931, 0.3119999999999998885 ) ) ;
#16634 = CARTESIAN_POINT ( 'NONE',  ( 0.2819296736111110979, 4.453555555631421470, -0.1167790944451423396 ) ) ;
#16635 = CARTESIAN_POINT ( 'NONE',  ( 0.1167790944451422702, 3.946611111186976384, -0.2819296736111110424 ) ) ;
#16636 = ORIENTED_EDGE ( 'NONE', *, *, #16780, .T. ) ;
#16637 = ORIENTED_EDGE ( 'NONE', *, *, #21241, .F. ) ;
#16638 = COORDINATED_UNIVERSAL_TIME_OFFSET ( 0, 0, .AHEAD. ) ;
#16639 = CARTESIAN_POINT ( 'NONE',  ( -0.3119999999999999996, 4.269527777777776478, -0.1292346314604056468 ) ) ;
#16640 = CARTESIAN_POINT ( 'NONE',  ( 0.05000000000000028727, 0.000000000000000000, -0.6280533563299045552 ) ) ;
#16641 = EDGE_CURVE ( 'NONE', #6063, #23807, #22081, .T. ) ;
#16642 = DIRECTION ( 'NONE',  ( 0.5000000000000004441, -0.8660254037844384856, 0.000000000000000000 ) ) ;
#16643 = ORIENTED_EDGE ( 'NONE', *, *, #6816, .F. ) ;
#16644 = CARTESIAN_POINT ( 'NONE',  ( 0.1292346314604056745, 0.5215277776260448528, -0.3119999999999999996 ) ) ;
#16645 = CIRCLE ( 'NONE', #5742, 0.1874999999999998335 ) ;
#16646 = DIRECTION ( 'NONE',  ( -0.000000000000000000, -1.000000000000000000, -0.000000000000000000 ) ) ;
#16647 = DIRECTION ( 'NONE',  ( 1.000000000000000000, 0.000000000000000000, 0.000000000000000000 ) ) ;
#16648 = CARTESIAN_POINT ( 'NONE',  ( 0.01934516033330287155, 5.167810441017906875, 0.2967713041391435991 ) ) ;
#16649 = EDGE_LOOP ( 'NONE', ( #10169, #9427, #23087, #7779 ) ) ;
#16650 = ORIENTED_EDGE ( 'NONE', *, *, #5716, .F. ) ;
#16651 = CARTESIAN_POINT ( 'NONE',  ( -0.2923287055106771337, 0.05446428561674331731, 0.2123892367102619971 ) ) ;
#16652 = DIRECTION ( 'NONE',  ( 0.4999999999999987788, 0.8660254037844393737, 0.000000000000000000 ) ) ;
#16653 = CARTESIAN_POINT ( 'NONE',  ( 0.2764156081756484196, -5.077672346800151106E-17, 0.2827777777777812362 ) ) ;
#16654 = CARTESIAN_POINT ( 'NONE',  ( -0.1167790944451423535, 4.196611111186976828, 0.2819296736111110424 ) ) ;
#16655 = CARTESIAN_POINT ( 'NONE',  ( 0.1993543840281267465, 5.151472222298087544, 0.1993543840281266633 ) ) ;
#16656 = CARTESIAN_POINT ( 'NONE',  ( 0.1459302940035057949, -0.2450006702336079423, 0.3966998585268076694 ) ) ;
#16657 = CARTESIAN_POINT ( 'NONE',  ( 0.3949999999999999623, 2.978485840173427324, -0.04999999999999915623 ) ) ;
#16658 = CARTESIAN_POINT ( 'NONE',  ( 0.1292346314604058410, 3.845916666666666206, 0.3119999999999998885 ) ) ;
#16659 = CARTESIAN_POINT ( 'NONE',  ( -0.2206173157302027676, 5.009111111262843252, 0.2206173157302028787 ) ) ;
#16660 = CARTESIAN_POINT ( 'NONE',  ( -0.1993543840281266910, 5.193138888964755395, -0.1993543840281266910 ) ) ;
#16661 = VECTOR ( 'NONE', #15954, 39.37007874015748143 ) ;
#16662 = CYLINDRICAL_SURFACE ( 'NONE', #10538, 0.3150000000000000022 ) ;
#16663 = EDGE_LOOP ( 'NONE', ( #3607, #20346, #17044, #21648 ) ) ;
#16664 = CARTESIAN_POINT ( 'NONE',  ( 0.2043171450904766873, 0.03871863473645468373, -0.2036093692351375051 ) ) ;
#16665 = VERTEX_POINT ( 'NONE', #23587 ) ;
#16666 = CARTESIAN_POINT ( 'NONE',  ( -0.2230971623002953874, 0.2230971623002954152, 0.2254861111111142458 ) ) ;
#16667 = CARTESIAN_POINT ( 'NONE',  ( -0.1167790944451423535, 5.196611111186976828, 0.2819296736111110424 ) ) ;
#16668 = VERTEX_POINT ( 'NONE', #3846 ) ;
#16669 = CARTESIAN_POINT ( 'NONE',  ( 0.3858656996964998642, -0.3184862117744570176, 0.4002370417399356284 ) ) ;
#16670 = CARTESIAN_POINT ( 'NONE',  ( 0.7847114317029997288, 2.291712385858714729, -0.8254988538245822127 ) ) ;
#16671 = CIRCLE ( 'NONE', #6150, 0.2499999999999999722 ) ;
#16672 = CARTESIAN_POINT ( 'NONE',  ( -0.2819296736111110979, 0.2402777777019112215, -0.1167790944451423396 ) ) ;
#16673 = CARTESIAN_POINT ( 'NONE',  ( 0.000000000000000000, 0.2764156081756484196, 0.1369444444444467002 ) ) ;
#16674 = EDGE_CURVE ( 'NONE', #12233, #15698, #3727, .T. ) ;
#16675 = CARTESIAN_POINT ( 'NONE',  ( 0.2819296736111110979, 5.005638888964754507, -3.452642723725051716E-17 ) ) ;
#16676 = CARTESIAN_POINT ( 'NONE',  ( 0.03527991335344082824, 4.487285812805300367, -0.3100400492211025094 ) ) ;
#16677 = ORIENTED_EDGE ( 'NONE', *, *, #8493, .T. ) ;
#16678 = EDGE_CURVE ( 'NONE', #8540, #549, #18820, .T. ) ;
#16679 = CARTESIAN_POINT ( 'NONE',  ( -0.1167790944451423535, 4.974388888964754507, 0.2819296736111110424 ) ) ;
#16680 = CARTESIAN_POINT ( 'NONE',  ( -0.4000000000000000222, 0.07321428551920090844, 0.1299678784931624920 ) ) ;
#16681 = CARTESIAN_POINT ( 'NONE',  ( -0.009623778223146972621, 4.266321329850166322, -0.3120828329435257342 ) ) ;
#16682 = DIRECTION ( 'NONE',  ( 0.000000000000000000, 0.000000000000000000, 1.000000000000000000 ) ) ;
#16683 = CARTESIAN_POINT ( 'NONE',  ( -0.3125000000000000000, 1.913510623667739771E-17, 0.1161111111111130384 ) ) ;
#16684 = PERSON ( 'NAUO-PER2', 'UNSPECIFIED', 'UNSPECIFIED', ('UNSPECIFIED'), ('UNSPECIFIED'), ('UNSPECIFIED') ) ;
#16685 = CARTESIAN_POINT ( 'NONE',  ( -0.1292346314604057023, 4.394527777777777366, 0.3119999999999998885 ) ) ;
#16686 = CARTESIAN_POINT ( 'NONE',  ( 0.1993543840281267465, 4.040361111186976828, 0.1993543840281266633 ) ) ;
#16687 = CYLINDRICAL_SURFACE ( 'NONE', #1533, 0.3125000000000000000 ) ;
#16688 = CARTESIAN_POINT ( 'NONE',  ( 0.2994861972273289985, 4.032443608799596291, -0.08761480198954196830 ) ) ;
#16689 = CARTESIAN_POINT ( 'NONE',  ( 0.2206173157302027676, 0.5041666665149336923, 0.2206173157302028787 ) ) ;
#16690 = ORIENTED_EDGE ( 'NONE', *, *, #15494, .F. ) ;
#16691 = CARTESIAN_POINT ( 'NONE',  ( -0.4593750000000004219, -0.2760455974562901482, 0.3779506566538942125 ) ) ;
#16692 = AXIS2_PLACEMENT_3D ( 'NONE', #12857, #11012, #15034 ) ;
#16693 = LINE ( 'NONE', #6068, #11962 ) ;
#16694 = CARTESIAN_POINT ( 'NONE',  ( 0.000000000000000000, 0.2764156081756484196, 0.1855555555555581937 ) ) ;
#16695 = DIRECTION ( 'NONE',  ( -0.8459207832372986902, -0.4883925919151528294, 0.2142211582677917003 ) ) ;
#16696 = CARTESIAN_POINT ( 'NONE',  ( -0.2494838521722312075, 4.452466089143981343, 0.1917547050432406863 ) ) ;
#16697 = APPROVAL ( #21638, 'UNSPECIFIED' ) ;
#16698 = FACE_OUTER_BOUND ( 'NONE', #2492, .T. ) ;
#16699 = CARTESIAN_POINT ( 'NONE',  ( -6.979263641208234666E-17, 0.2794642856167432465, 0.3799334167787516425 ) ) ;
#16700 = CARTESIAN_POINT ( 'NONE',  ( 0.1167790944451423257, 0.3236111110352444808, -0.2819296736111110424 ) ) ;
#16701 = CARTESIAN_POINT ( 'NONE',  ( 0.001115507632757668918, 3.877136689224211175, -0.3119982913588789653 ) ) ;
#16702 = FACE_OUTER_BOUND ( 'NONE', #12934, .T. ) ;
#16703 = CARTESIAN_POINT ( 'NONE',  ( 5.731347020009612645E-17, 3.842444444444443441, 0.3119999999999999996 ) ) ;
#16704 = CARTESIAN_POINT ( 'NONE',  ( -3.385114897866767815E-17, -0.2764156081756484196, -0.1130555555555552844 ) ) ;
#16705 = VERTEX_POINT ( 'NONE', #14470 ) ;
#16706 = ORIENTED_EDGE ( 'NONE', *, *, #24084, .F. ) ;
#16707 = CARTESIAN_POINT ( 'NONE',  ( -0.2122204171184600696, 5.098494865722095426, -0.2275089404706317764 ) ) ;
#16708 = CARTESIAN_POINT ( 'NONE',  ( 0.4581189881604794123, -0.2644951211353317455, 0.3941886329748525153 ) ) ;
#16709 = CARTESIAN_POINT ( 'NONE',  ( -0.1292346314604058410, 0.05624999999999965444, 0.3119999999999998885 ) ) ;
#16710 = CARTESIAN_POINT ( 'NONE',  ( 0.3119999999999999996, 5.082027777777776478, -0.1292346314604056745 ) ) ;
#16711 = AXIS2_PLACEMENT_3D ( 'NONE', #23369, #23486, #6802 ) ;
#16712 = CARTESIAN_POINT ( 'NONE',  ( -0.2233192592356399997, 0.2723214284738861291, 0.3073725909049499494 ) ) ;
#16713 = CARTESIAN_POINT ( 'NONE',  ( -0.1993543840281266910, 4.526472222298087544, -0.1993543840281266910 ) ) ;
#16714 = CARTESIAN_POINT ( 'NONE',  ( -0.001863919267159286786, 4.559812086079793048, -2.908070964936878333 ) ) ;
#16715 = CARTESIAN_POINT ( 'NONE',  ( -0.2206173157302027676, 4.391055555555555046, 0.2206173157302028787 ) ) ;
#16716 = EDGE_CURVE ( 'NONE', #17904, #22501, #6599, .T. ) ;
#16717 = EDGE_LOOP ( 'NONE', ( #7617, #21635, #764, #6151 ) ) ;
#16718 = CARTESIAN_POINT ( 'NONE',  ( 0.2695900040198371261, 4.368010068071540353, -0.1590464363266536896 ) ) ;
#16719 = CARTESIAN_POINT ( 'NONE',  ( -0.2819296736111110979, 5.019527777853642903, 0.000000000000000000 ) ) ;
#16720 = CARTESIAN_POINT ( 'NONE',  ( -0.2990480016229275506, 5.156380186802008936, 0.03674222046541380376 ) ) ;
#16721 = DIRECTION ( 'NONE',  ( 0.2508162484481474830, -0.9659258262890726421, -0.06386319458161507367 ) ) ;
#16722 = CARTESIAN_POINT ( 'NONE',  ( 0.3999999999999999667, 0.2517857140906293867, -0.1299678784931625197 ) ) ;
#16723 = VECTOR ( 'NONE', #4922, 39.37007874015748143 ) ;
#16724 = CARTESIAN_POINT ( 'NONE',  ( 0.2819296736111110979, 4.606333333409200037, -0.1167790944451423396 ) ) ;
#16725 = PERSON_AND_ORGANIZATION ( #5616, #9991 ) ;
#16726 = CARTESIAN_POINT ( 'NONE',  ( -0.4593749999999912070, 0.2760455974562950887, 0.06112444011295854046 ) ) ;
#16727 = PLANE ( 'NONE',  #11656 ) ;
#16728 = CARTESIAN_POINT ( 'NONE',  ( 0.1167790944451423257, 0.5597222221463556968, -0.2819296736111110424 ) ) ;
#16729 = ORIENTED_EDGE ( 'NONE', *, *, #6958, .T. ) ;
#16730 = EDGE_LOOP ( 'NONE', ( #12131, #3394, #5236, #10942 ) ) ;
#16731 = CARTESIAN_POINT ( 'NONE',  ( 0.2819296736111110424, 0.2680555554796889561, 0.1167790944451424923 ) ) ;
#16732 = CARTESIAN_POINT ( 'NONE',  ( -0.03785093491744839778, 4.711555345668029027, -0.3099667384353548827 ) ) ;
#16733 = CARTESIAN_POINT ( 'NONE',  ( -0.3236067977499789694, 0.2857142857142855874, -0.2351141009169893104 ) ) ;
#16734 = CARTESIAN_POINT ( 'NONE',  ( 0.3155070326520292845, -5.795770164686806123E-17, -0.07659722222222187238 ) ) ;
#16735 = CARTESIAN_POINT ( 'NONE',  ( 0.6033333333333333881, 2.873333333333333517, -2.382666666666667155 ) ) ;
#16736 = CARTESIAN_POINT ( 'NONE',  ( -0.3109939306932527070, 3.891914723735419912, 0.03129033405693151804 ) ) ;
#16737 = CARTESIAN_POINT ( 'NONE',  ( -0.1167790944451422702, 0.1638888888130222432, -0.2819296736111110979 ) ) ;
#16738 = CARTESIAN_POINT ( 'NONE',  ( 0.9287197593527887207, 2.340128234365810300, -1.330304951501487754 ) ) ;
#16739 = CARTESIAN_POINT ( 'NONE',  ( 5.178964085587577574E-17, 4.602861111186976828, 0.2819296736111110979 ) ) ;
#16740 = ORIENTED_EDGE ( 'NONE', *, *, #6207, .T. ) ;
#16741 = CARTESIAN_POINT ( 'NONE',  ( -0.2472135954999579444, 0.1303571426620580842, -0.3402603233408159622 ) ) ;
#16742 = CARTESIAN_POINT ( 'NONE',  ( 0.1125251556717559304, 1.376365001936862257E-16, -0.3585253126667320434 ) ) ;
#16743 = CARTESIAN_POINT ( 'NONE',  ( -0.1993543840281266910, 5.026472222298088433, -0.1993543840281266910 ) ) ;
#16744 = CARTESIAN_POINT ( 'NONE',  ( -0.2819296736111110424, 4.356333333409198261, 0.1167790944451424923 ) ) ;
#16745 = CARTESIAN_POINT ( 'NONE',  ( 1.519200945994765378E-06, 3.766055514889470324, -0.3119999999963013471 ) ) ;
#16746 = DIRECTION ( 'NONE',  ( 0.8660254037844434816, 0.000000000000000000, -0.4999999999999915068 ) ) ;
#16747 = AXIS2_PLACEMENT_3D ( 'NONE', #21014, #4308, #2494 ) ;
#16748 = CARTESIAN_POINT ( 'NONE',  ( 0.000000000000000000, 0.000000000000000000, 0.000000000000000000 ) ) ;
#16749 = CARTESIAN_POINT ( 'NONE',  ( 5.731347020009612645E-17, 4.182722222373953969, 0.3119999999999999996 ) ) ;
#16750 = CARTESIAN_POINT ( 'NONE',  ( 0.2819296736111111534, 4.446611111186976828, 0.1167790944451422563 ) ) ;
#16751 = CARTESIAN_POINT ( 'NONE',  ( -0.3103034095256952951, 0.3621121203451553860, 0.4135550951626318361 ) ) ;
#16752 = CARTESIAN_POINT ( 'NONE',  ( 0.1338087529396776443, -0.2734308413693284923, -0.09311885657517415815 ) ) ;
#16753 = VERTEX_POINT ( 'NONE', #14838 ) ;
#16754 = ORIENTED_EDGE ( 'NONE', *, *, #16674, .F. ) ;
#16755 = COORDINATED_UNIVERSAL_TIME_OFFSET ( 0, 0, .AHEAD. ) ;
#16756 = EDGE_CURVE ( 'NONE', #23659, #23361, #16537, .T. ) ;
#16757 = VECTOR ( 'NONE', #21548, 39.37007874015748143 ) ;
#16758 = CARTESIAN_POINT ( 'NONE',  ( -0.1158813573290139315, 4.846026232838027248, 0.2897518779968182856 ) ) ;
#16759 = DIRECTION ( 'NONE',  ( -1.000000000000000000, 0.000000000000000000, 4.440892098500625176E-16 ) ) ;
#16760 = EDGE_LOOP ( 'NONE', ( #8199, #16360, #15944, #20488, #20327 ) ) ;
#16761 = CARTESIAN_POINT ( 'NONE',  ( -0.1292346314604056190, 0.4173611109593781676, -0.3119999999999999996 ) ) ;
#16762 = VERTEX_POINT ( 'NONE', #7270 ) ;
#16763 = DIRECTION ( 'NONE',  ( 0.000000000000000000, 0.000000000000000000, -1.000000000000000000 ) ) ;
#16764 = CARTESIAN_POINT ( 'NONE',  ( -0.2005194665486881855, 3.716698251689450672, -0.2390317579944993553 ) ) ;
#16765 = CARTESIAN_POINT ( 'NONE',  ( 0.2233192592356399997, 0.004464285616743319737, -0.3073725909049500049 ) ) ;
#16766 = CARTESIAN_POINT ( 'NONE',  ( -5.731347020009612645E-17, 0.5041666666666663188, 0.3119999999999999996 ) ) ;
#16767 = VERTEX_POINT ( 'NONE', #5551 ) ;
#16768 = CARTESIAN_POINT ( 'NONE',  ( 0.1116596296178199860, 0.09732142847388618179, -0.3436530038418508792 ) ) ;
#16769 = DIRECTION ( 'NONE',  ( 0.2610779533529330454, 0.003182690398834837290, 0.9653124741527318031 ) ) ;
#16770 = CARTESIAN_POINT ( 'NONE',  ( -0.1954553509668046918, -0.1954553509668046640, 0.3175000000000037237 ) ) ;
#16771 = CARTESIAN_POINT ( 'NONE',  ( 0.2819296736111110424, 4.328555555631420582, -0.1167790944451423396 ) ) ;
#16772 = CARTESIAN_POINT ( 'NONE',  ( 0.1167790944451422702, 5.168833333409199149, -0.2819296736111110979 ) ) ;
#16773 = CARTESIAN_POINT ( 'NONE',  ( -0.1380212367034723275, -0.4615792792006397915, 0.4105854900893666226 ) ) ;
#16774 = CARTESIAN_POINT ( 'NONE',  ( 0.3125000000000000000, -5.740531871003217465E-17, 0.2550000000000030020 ) ) ;
#16775 = CARTESIAN_POINT ( 'NONE',  ( 0.2206173157302028787, 3.904944444444443885, 0.2206173157302027954 ) ) ;
#16776 = CARTESIAN_POINT ( 'NONE',  ( 5.731347020009612645E-17, 4.849388889040620931, 0.3119999999999999996 ) ) ;
#16777 = CARTESIAN_POINT ( 'NONE',  ( -1.726321361862525858E-17, 5.186194444520309865, -0.2819296736111110979 ) ) ;
#16778 =( BOUNDED_CURVE ( )  B_SPLINE_CURVE ( 2, ( #3649, #5110, #20242, #16583, #16344, #23875, #3531, #24121, #9261 ),
 .UNSPECIFIED., .F., .T. ) 
 B_SPLINE_CURVE_WITH_KNOTS ( ( 3, 2, 2, 2, 3 ),
 ( 0.8958333333333333703, 0.9062500000000000000, 0.9166666666666666297, 0.9270833333333333703, 0.9375000000000000000 ),
 .UNSPECIFIED. ) 
 CURVE ( )  GEOMETRIC_REPRESENTATION_ITEM ( )  RATIONAL_B_SPLINE_CURVE ( ( 1.000000000000000000, 0.9238795325112867385, 1.000000000000000000, 0.9238795325112867385, 1.000000000000000000, 0.9238795325112867385, 1.000000000000000000, 0.9238795325112867385, 1.000000000000000000 ) ) 
 REPRESENTATION_ITEM ( '' )  );
#16779 = AXIS2_PLACEMENT_3D ( 'NONE', #17419, #7901, #4250 ) ;
#16780 = EDGE_CURVE ( 'NONE', #9037, #6959, #13369, .T. ) ;
#16781 = EDGE_CURVE ( 'NONE', #16373, #7491, #1293, .T. ) ;
#16782 = VECTOR ( 'NONE', #13048, 39.37007874015748143 ) ;
#16783 = ADVANCED_FACE ( 'NONE', ( #3481 ), #6491, .T. ) ;
#16784 = CARTESIAN_POINT ( 'NONE',  ( 0.3119999999999999996, 0.4104166666666663188, -0.1292346314604056468 ) ) ;
#16785 = VERTEX_POINT ( 'NONE', #16888 ) ;
#16786 = CARTESIAN_POINT ( 'NONE',  ( -0.3613381517857143788, 0.03303571418817188854, 0.1174058825155740310 ) ) ;
#16787 = CARTESIAN_POINT ( 'NONE',  ( 0.2658661084243346684, 0.03242967361111057795, 0.09380593400082704036 ) ) ;
#16788 = CALENDAR_DATE ( 2026, 7, 10 ) ;
#16789 = EDGE_CURVE ( 'NONE', #18459, #14583, #4201, .T. ) ;
#16790 = FACE_OUTER_BOUND ( 'NONE', #11911, .T. ) ;
#16791 = CARTESIAN_POINT ( 'NONE',  ( 5.178964085587577574E-17, 5.200083333409199149, 0.2819296736111110979 ) ) ;
#16792 = CARTESIAN_POINT ( 'NONE',  ( 0.2819296736111111534, 3.779944444520309865, 0.1167790944451422563 ) ) ;
#16793 = DIRECTION ( 'NONE',  ( 0.000000000000000000, 0.000000000000000000, -1.000000000000000000 ) ) ;
#16794 = CARTESIAN_POINT ( 'NONE',  ( 0.3613381517857143232, 0.3473214284738860291, 0.1174058825155742114 ) ) ;
#16795 = VECTOR ( 'NONE', #8819, 39.37007874015748143 ) ;
#16796 = EDGE_LOOP ( 'NONE', ( #22842, #6755, #8982, #20065, #4181 ) ) ;
#16797 = CARTESIAN_POINT ( 'NONE',  ( 0.000000000000000000, 0.2764156081756484196, 0.07444444444444621445 ) ) ;
#16798 = CARTESIAN_POINT ( 'NONE',  ( -0.1993543840281266633, 0.3479166665908000056, -0.1993543840281266910 ) ) ;
#16799 = CARTESIAN_POINT ( 'NONE',  ( -0.2764156081756484196, 1.692557448933383907E-17, 0.3175000000000036682 ) ) ;
#16800 = CARTESIAN_POINT ( 'NONE',  ( -0.2819296736111110424, 5.029944444520310753, -0.1167790944451423119 ) ) ;
#16801 = CARTESIAN_POINT ( 'NONE',  ( -0.4805070082343984583, -0.2560807851245831546, 0.04413116910601652676 ) ) ;
#16802 = EDGE_CURVE ( 'NONE', #13969, #18530, #20906, .T. ) ;
#16803 = CARTESIAN_POINT ( 'NONE',  ( -0.2819296736111110424, 4.849388888964755395, -0.1167790944451423119 ) ) ;
#16804 = DIRECTION ( 'NONE',  ( 0.000000000000000000, 0.000000000000000000, -1.000000000000000000 ) ) ;
#16805 = CARTESIAN_POINT ( 'NONE',  ( 0.000000000000000000, 0.8699999999999998845, 0.000000000000000000 ) ) ;
#16806 = LINE ( 'NONE', #9241, #12977 ) ;
#16807 = CARTESIAN_POINT ( 'NONE',  ( 1.655695048498512678, 2.340128234365810744, -2.057280240647211489 ) ) ;
#16808 = CARTESIAN_POINT ( 'NONE',  ( 0.2206173157302027954, 4.585499999999999687, -0.2206173157302028232 ) ) ;
#16809 = CARTESIAN_POINT ( 'NONE',  ( 5.178964085587577574E-17, 3.866750000075865668, 0.2819296736111110979 ) ) ;
#16810 = CARTESIAN_POINT ( 'NONE',  ( -0.1060554323913586589, 3.514980167629567998, 2.783525011231007706 ) ) ;
#16811 = CARTESIAN_POINT ( 'NONE',  ( 0.1888842787674890333, 4.021839019550402128, 0.2483332517396733830 ) ) ;
#16812 = CARTESIAN_POINT ( 'NONE',  ( 2.570936052289255124E-07, 3.738287934957344127, 0.3119999999997750129 ) ) ;
#16813 = ORIENTED_EDGE ( 'NONE', *, *, #14678, .T. ) ;
#16814 = DIRECTION ( 'NONE',  ( 0.000000000000000000, 1.000000000000000000, 0.000000000000000000 ) ) ;
#16815 = CARTESIAN_POINT ( 'NONE',  ( -0.07559737730188846594, 4.101573950995675233, -0.3050544060259108292 ) ) ;
#16816 = EDGE_CURVE ( 'NONE', #10130, #23979, #20786, .T. ) ;
#16817 = ADVANCED_FACE ( 'NONE', ( #22735 ), #15310, .F. ) ;
#16818 = CARTESIAN_POINT ( 'NONE',  ( 0.3018713704988151836, 4.638800393405135836, 0.08078439495390804526 ) ) ;
#16819 = CARTESIAN_POINT ( 'NONE',  ( -0.2764156081756484196, 0.1144950937579609918, 0.1959722222222249899 ) ) ;
#16820 = CARTESIAN_POINT ( 'NONE',  ( -0.3125000000000000000, 3.738758431839877614E-19, -0.1016666666666665164 ) ) ;
#16821 = DIRECTION ( 'NONE',  ( 0.000000000000000000, 1.000000000000000000, 0.000000000000000000 ) ) ;
#16822 =( BOUNDED_CURVE ( )  B_SPLINE_CURVE ( 2, ( #7887, #15339, #4234, #11686, #9856, #18752, #14982, #216, #15104, #19111, #5819, #2414, #23230 ),
 .UNSPECIFIED., .F., .T. ) 
 B_SPLINE_CURVE_WITH_KNOTS ( ( 3, 2, 2, 2, 2, 2, 3 ),
 ( 0.7500000000000000000, 0.7571428571428571175, 0.7714285714285714635, 0.7857142857142856984, 0.8000000000000000444, 0.8142857142857142794, 0.8214285714285715079 ),
 .UNSPECIFIED. ) 
 CURVE ( )  GEOMETRIC_REPRESENTATION_ITEM ( )  RATIONAL_B_SPLINE_CURVE ( ( 0.9755282581475768211, 0.9755282581475768211, 1.000000000000000000, 0.9510565162951535312, 1.000000000000000000, 0.9510565162951535312, 1.000000000000000000, 0.9510565162951535312, 1.000000000000000000, 0.9510565162951535312, 1.000000000000000000, 0.9755282581475765991, 0.9755282581475768211 ) ) 
 REPRESENTATION_ITEM ( '' )  );
#16823 = EDGE_LOOP ( 'NONE', ( #16650, #13234, #1705 ) ) ;
#16824 = CARTESIAN_POINT ( 'NONE',  ( 0.3613381517857143232, 0.3687499999024574926, 0.000000000000000000 ) ) ;
#16825 = CARTESIAN_POINT ( 'NONE',  ( -0.1167790944451424368, 0.2958333332574667462, 0.2819296736111110424 ) ) ;
#16826 = CARTESIAN_POINT ( 'NONE',  ( 0.3119994934711425860, 3.862180426189363303, 0.04084270294850755878 ) ) ;
#16827 = CARTESIAN_POINT ( 'NONE',  ( 1.750236327630675475E-17, 0.05178571409062948661, -0.3999999999999999667 ) ) ;
#16828 = CARTESIAN_POINT ( 'NONE',  ( 0.7919466436700954848, 2.740039370078740433, -2.986000000000000210 ) ) ;
#16829 = CARTESIAN_POINT ( 'NONE',  ( -0.1144950937579609779, 0.2764156081756484196, 0.02930555555555695163 ) ) ;
#16830 = CARTESIAN_POINT ( 'NONE',  ( 0.000000000000000000, 5.954200000000001936, 0.000000000000000000 ) ) ;
#16831 = CARTESIAN_POINT ( 'NONE',  ( -0.3119999999999999996, 4.717444444444443441, 0.000000000000000000 ) ) ;
#16832 = CARTESIAN_POINT ( 'NONE',  ( -0.2206173157302027954, 0.09444444444444409503, -0.2206173157302028232 ) ) ;
#16833 = CARTESIAN_POINT ( 'NONE',  ( 5.731347020009612645E-17, 5.175777777777777366, 0.3119999999999999996 ) ) ;
#16834 = CARTESIAN_POINT ( 'NONE',  ( -0.1116596296178199582, 0.1758928570453147100, -0.3436530038418508792 ) ) ;
#16835 = CARTESIAN_POINT ( 'NONE',  ( 0.1167790944451422702, 4.293833333409199149, -0.2819296736111110424 ) ) ;
#16836 = CARTESIAN_POINT ( 'NONE',  ( 0.000000000000000000, 5.384999999999999787, 0.000000000000000000 ) ) ;
#16837 = CARTESIAN_POINT ( 'NONE',  ( 0.3532795013362199366, 1.447158556123030133E-17, -0.07948650416438482469 ) ) ;
#16838 = ORIENTED_EDGE ( 'NONE', *, *, #23894, .F. ) ;
#16839 = CARTESIAN_POINT ( 'NONE',  ( 0.04809061687855835376, 4.375824664982923551, -0.3084196734384360150 ) ) ;
#16840 = CARTESIAN_POINT ( 'NONE',  ( 0.2819296736111110979, 5.043833333409199149, 0.1167790944451422425 ) ) ;
#16841 = CARTESIAN_POINT ( 'NONE',  ( -0.2911615289334776868, 5.153441331032047046, -0.08051819117923980640 ) ) ;
#16842 = EDGE_CURVE ( 'NONE', #9466, #21724, #502, .T. ) ;
#16843 = CARTESIAN_POINT ( 'NONE',  ( -0.1292346314604056190, 0.2020833333333329207, -0.3119999999999999996 ) ) ;
#16844 = CARTESIAN_POINT ( 'NONE',  ( -0.1993543840281266355, 4.637583333409198261, 0.1993543840281267465 ) ) ;
#16845 = CONTEXT_DEPENDENT_SHAPE_REPRESENTATION ( #12184, #12876 ) ;
#16846 = CYLINDRICAL_SURFACE ( 'NONE', #8990, 0.2109499999999996656 ) ;
#16847 = FACE_OUTER_BOUND ( 'NONE', #18934, .T. ) ;
#16848 = CARTESIAN_POINT ( 'NONE',  ( -0.1993543840281267465, 0.5840277777019110550, 0.1993543840281266633 ) ) ;
#16849 = VERTEX_POINT ( 'NONE', #4317 ) ;
#16850 = CARTESIAN_POINT ( 'NONE',  ( 0.2819296736111110424, 0.2194444443685777957, -0.1167790944451423119 ) ) ;
#16851 = CARTESIAN_POINT ( 'NONE',  ( -0.05329418186030111804, -0.01080343630441895492, 2.905739844640345293 ) ) ;
#16852 = CARTESIAN_POINT ( 'NONE',  ( -0.3236067977499790249, 0.005357142662058056448, 0.2351141009169892271 ) ) ;
#16853 = CARTESIAN_POINT ( 'NONE',  ( 0.2472135954999579166, 0.3178571428571427826, 0.3402603233408160732 ) ) ;
#16854 = CARTESIAN_POINT ( 'NONE',  ( 0.000000000000000000, 0.3155070326520292845, 0.04840277777777911294 ) ) ;
#16855 = VECTOR ( 'NONE', #17664, 39.37007874015748143 ) ;
#16856 = CARTESIAN_POINT ( 'NONE',  ( -0.01172578639831953380, -0.5344959914317446437, 0.04874733047933992036 ) ) ;
#16857 = EDGE_CURVE ( 'NONE', #10945, #20425, #15072, .T. ) ;
#16858 = DIRECTION ( 'NONE',  ( -0.8660254037844388186, 0.4999999999999997224, 0.000000000000000000 ) ) ;
#16859 = CARTESIAN_POINT ( 'NONE',  ( 0.1993543840281266355, 0.3062499999241333759, 0.1993543840281267465 ) ) ;
#16860 = CARTESIAN_POINT ( 'NONE',  ( -5.178964085587577574E-17, 0.07708333325746669074, 0.2819296736111110979 ) ) ;
#16861 = CARTESIAN_POINT ( 'NONE',  ( -1.726321361862525858E-17, 4.186194444520309865, -0.2819296736111110979 ) ) ;
#16862 = CARTESIAN_POINT ( 'NONE',  ( -0.3999999999999999667, 0.06607142837634377708, -0.1299678784931626030 ) ) ;
#16863 = CARTESIAN_POINT ( 'NONE',  ( 5.178964085587577574E-17, 4.769527777853643791, 0.2819296736111110979 ) ) ;
#16864 = CARTESIAN_POINT ( 'NONE',  ( -0.1993543840281266355, 4.470916666742532186, 0.1993543840281267465 ) ) ;
#16865 = DIRECTION ( 'NONE',  ( 0.000000000000000000, 0.000000000000000000, -1.000000000000000000 ) ) ;
#16866 = CARTESIAN_POINT ( 'NONE',  ( -1.910449006669871087E-17, 5.036888888888888971, -0.3119999999999999996 ) ) ;
#16867 = CC_DESIGN_DATE_AND_TIME_ASSIGNMENT ( #17472, #1006, ( #15678 ) ) ;
#16868 = CARTESIAN_POINT ( 'NONE',  ( -0.1292346314604057023, 4.179250000151731648, 0.3119999999999998885 ) ) ;
#16869 = CARTESIAN_POINT ( 'NONE',  ( 0.000000000000000000, 0.1799999999999999933, 0.000000000000000000 ) ) ;
#16870 = EDGE_LOOP ( 'NONE', ( #11166, #12625, #18253, #22049 ) ) ;
#16871 = ORIENTED_EDGE ( 'NONE', *, *, #4976, .T. ) ;
#16872 = COORDINATED_UNIVERSAL_TIME_OFFSET ( 0, 0, .AHEAD. ) ;
#16873 = CARTESIAN_POINT ( 'NONE',  ( 0.4621660567954134491, -0.2744341800641368345, 0.05971082423030580483 ) ) ;
#16874 = DIRECTION ( 'NONE',  ( 0.000000000000000000, -0.9961946980917454342, -0.08715574274765833240 ) ) ;
#16875 = LINE ( 'NONE', #20651, #17862 ) ;
#16876 = ORIENTED_EDGE ( 'NONE', *, *, #2572, .F. ) ;
#16877 = CARTESIAN_POINT ( 'NONE',  ( -0.2206173157302027954, 0.5319444442927114824, -0.2206173157302028232 ) ) ;
#16878 = LINE ( 'NONE', #11162, #3506 ) ;
#16879 = CARTESIAN_POINT ( 'NONE',  ( 0.1358625382851928742, 4.742203176482449933, 0.2831117945823172222 ) ) ;
#16880 = CARTESIAN_POINT ( 'NONE',  ( -0.3613381517857144343, 0.03303571418817188854, 0.1174058825155740171 ) ) ;
#16881 = CARTESIAN_POINT ( 'NONE',  ( 0.3039879257364922482, 3.976659419480376823, -0.08128067288674797886 ) ) ;
#16882 = ORIENTED_EDGE ( 'NONE', *, *, #3305, .F. ) ;
#16883 = CARTESIAN_POINT ( 'NONE',  ( -0.3613381517857143232, 0.1187499999024576036, -4.425116109941954795E-17 ) ) ;
#16884 = DIRECTION ( 'NONE',  ( 0.000000000000000000, 0.000000000000000000, -1.000000000000000000 ) ) ;
#16885 = CARTESIAN_POINT ( 'NONE',  ( -0.2206173157302027676, 4.057722222222221120, 0.2206173157302028787 ) ) ;
#16886 = AXIS2_PLACEMENT_3D ( 'NONE', #15015, #22437, #18659 ) ;
#16887 = CARTESIAN_POINT ( 'NONE',  ( 0.1167790944451424368, 4.148000000075866112, 0.2819296736111110424 ) ) ;
#16888 = CARTESIAN_POINT ( 'NONE',  ( -0.4593750000000004219, 0.2760455974562897596, 0.3779506566538943790 ) ) ;
#16889 = CARTESIAN_POINT ( 'NONE',  ( 0.1586325827338087857, -0.4496793130216646950, 0.08858683671056813425 ) ) ;
#16890 = CARTESIAN_POINT ( 'NONE',  ( 0.3119999999999999996, 3.797305555555555046, 0.1292346314604056190 ) ) ;
#16891 = CARTESIAN_POINT ( 'NONE',  ( 0.2206173157302028787, 4.800777777929509327, 0.2206173157302027954 ) ) ;
#16892 = EDGE_CURVE ( 'NONE', #12518, #14569, #15426, .T. ) ;
#16893 = CARTESIAN_POINT ( 'NONE',  ( 5.178964085587577574E-17, 5.102861111186976828, 0.2819296736111110979 ) ) ;
#16894 = CARTESIAN_POINT ( 'NONE',  ( 0.2819296736111110424, 4.328555555631420582, -0.1167790944451423396 ) ) ;
#16895 = CARTESIAN_POINT ( 'NONE',  ( 0.3119999999999999996, 0.4069444444444440534, 0.000000000000000000 ) ) ;
#16896 = ORIENTED_EDGE ( 'NONE', *, *, #6639, .F. ) ;
#16897 = CARTESIAN_POINT ( 'NONE',  ( -0.2923287055106771337, 0.03660714275960045422, 0.2123892367102619971 ) ) ;
#16898 = CARTESIAN_POINT ( 'NONE',  ( 0.1792189426095378846, 0.03935871358545873361, -0.2268249990278165540 ) ) ;
#16899 = VERTEX_POINT ( 'NONE', #5908 ) ;
#16900 = CALENDAR_DATE ( 2026, 7, 10 ) ;
#16901 = VECTOR ( 'NONE', #13894, 39.37007874015748854 ) ;
#16902 = DIRECTION ( 'NONE',  ( 0.000000000000000000, -1.000000000000000000, -0.000000000000000000 ) ) ;
#16903 = CARTESIAN_POINT ( 'NONE',  ( -0.2819296736111110424, 5.078555555631420582, 0.1167790944451424923 ) ) ;
#16904 = CARTESIAN_POINT ( 'NONE',  ( 5.178964085587577574E-17, 3.936194444520310309, 0.2819296736111110979 ) ) ;
#16905 = CARTESIAN_POINT ( 'NONE',  ( 0.06940672806685913021, 4.406896202175514254, 0.3041826934043310171 ) ) ;
#16906 = CARTESIAN_POINT ( 'NONE',  ( -0.2233192592356399997, 0.3973214284738861291, 0.3073725909049499494 ) ) ;
#16907 = EDGE_CURVE ( 'NONE', #6119, #2426, #7765, .T. ) ;
#16908 = CARTESIAN_POINT ( 'NONE',  ( -0.1144950937579609779, 0.2764156081756484196, 0.07791666666666846597 ) ) ;
#16909 = CARTESIAN_POINT ( 'NONE',  ( -0.1993543840281267465, 0.4729166665907999501, 0.1993543840281266633 ) ) ;
#16910 = CARTESIAN_POINT ( 'NONE',  ( 0.1144950937579609085, -0.2764156081756484751, -0.1165277777777775636 ) ) ;
#16911 = CARTESIAN_POINT ( 'NONE',  ( -0.1167790944451423257, 4.967444444520310753, -0.2819296736111110424 ) ) ;
#16912 = DIRECTION ( 'NONE',  ( -1.000000000000000000, 0.000000000000000000, 0.000000000000000000 ) ) ;
#16913 = CARTESIAN_POINT ( 'NONE',  ( -0.2819296736111110424, 4.800777777853643791, 0.1167790944451424923 ) ) ;
#16914 = CARTESIAN_POINT ( 'NONE',  ( -0.04072741636813891064, 4.181569250771618229, 0.3099999491876047619 ) ) ;
#16915 = FACE_OUTER_BOUND ( 'NONE', #16870, .T. ) ;
#16916 = DIRECTION ( 'NONE',  ( 0.08715574274765830465, -0.9961946980917454342, -3.870492493070289564E-17 ) ) ;
#16917 = CARTESIAN_POINT ( 'NONE',  ( 0.3125000000000000000, -5.740531871003217465E-17, 0.09527777777777987622 ) ) ;
#16918 = CARTESIAN_POINT ( 'NONE',  ( 0.1292346314604058410, 4.512583333333332725, 0.3119999999999998885 ) ) ;
#16919 = CARTESIAN_POINT ( 'NONE',  ( -1.726321361862525858E-17, 3.838972222298087544, -0.2819296736111110979 ) ) ;
#16920 = VECTOR ( 'NONE', #4656, 39.37007874015748143 ) ;
#16921 = DIRECTION ( 'NONE',  ( -0.000000000000000000, 1.000000000000000000, 0.000000000000000000 ) ) ;
#16922 = EDGE_CURVE ( 'NONE', #19560, #6274, #9804, .T. ) ;
#16923 = CARTESIAN_POINT ( 'NONE',  ( 0.005285943416724413202, 4.988126182262142549, -0.3119616049321576323 ) ) ;
#16924 = DIRECTION ( 'NONE',  ( -0.000000000000000000, -1.000000000000000000, -0.000000000000000000 ) ) ;
#16925 = LINE ( 'NONE', #2298, #7000 ) ;
#16926 = ORIENTED_EDGE ( 'NONE', *, *, #16153, .F. ) ;
#16927 = AXIS2_PLACEMENT_3D ( 'NONE', #10881, #7335, #23776 ) ;
#16928 = CARTESIAN_POINT ( 'NONE',  ( -0.2854338313968505791, 4.109616874731887748, -0.1273923718972508889 ) ) ;
#16929 = CARTESIAN_POINT ( 'NONE',  ( 0.005393248022499976500, 4.654789771038872814, -0.3119600307737797618 ) ) ;
#16930 = CARTESIAN_POINT ( 'NONE',  ( -0.1144950937579609779, 0.2764156081756484196, 0.3556944444444484765 ) ) ;
#16931 = AXIS2_PLACEMENT_3D ( 'NONE', #7814, #4510, #4272 ) ;
#16932 = CARTESIAN_POINT ( 'NONE',  ( 1.645216030923674522, 2.291712385858714729, -2.498788568296995916 ) ) ;
#16933 = DIRECTION ( 'NONE',  ( 0.4999999999999916733, -0.000000000000000000, 0.8660254037844432595 ) ) ;
#16934 = ORIENTED_EDGE ( 'NONE', *, *, #4380, .T. ) ;
#16935 = CARTESIAN_POINT ( 'NONE',  ( -0.3613381517857143232, 0.1866071427596003585, -0.1174058825155741004 ) ) ;
#16936 = CARTESIAN_POINT ( 'NONE',  ( -0.2819296736111110424, 0.5041666665908000056, -0.1167790944451423396 ) ) ;
#16937 = CARTESIAN_POINT ( 'NONE',  ( -0.3125000000000004996, 0.1294417382415917195, 0.1751388888888916473 ) ) ;
#16938 = CARTESIAN_POINT ( 'NONE',  ( 0.4723904922468885048, -0.2801879233228460331, 0.04193467568257214922 ) ) ;
#16939 = LINE ( 'NONE', #22549, #15220 ) ;
#16940 = CARTESIAN_POINT ( 'NONE',  ( -0.2764156081756484196, -0.1144950937579609362, 0.2098611111111139405 ) ) ;
#16941 = CARTESIAN_POINT ( 'NONE',  ( -0.2466418311916984407, 5.099818558436279403, -0.1902706867175692762 ) ) ;
#16942 = CC_DESIGN_APPROVAL ( #2844, ( #12686 ) ) ;
#16943 = CARTESIAN_POINT ( 'NONE',  ( 0.3119999999999999996, 0.2437499999999996891, -0.1292346314604056468 ) ) ;
#16944 = CARTESIAN_POINT ( 'NONE',  ( -1.910449006669871087E-17, 5.147999999999998799, -0.3119999999999999996 ) ) ;
#16945 = CARTESIAN_POINT ( 'NONE',  ( -0.1993543840281266910, 4.248694444520310753, -0.1993543840281266910 ) ) ;
#16946 = EDGE_CURVE ( 'NONE', #22384, #20123, #19924, .T. ) ;
#16947 = PLANE ( 'NONE',  #4594 ) ;
#16948 = CARTESIAN_POINT ( 'NONE',  ( 0.2472135954999579721, 0.4017857140906294644, -0.3402603233408160732 ) ) ;
#16949 = VERTEX_POINT ( 'NONE', #4792 ) ;
#16950 = ORIENTED_EDGE ( 'NONE', *, *, #15637, .T. ) ;
#16951 = DIRECTION ( 'NONE',  ( 0.000000000000000000, 0.000000000000000000, -1.000000000000000000 ) ) ;
#16952 = CARTESIAN_POINT ( 'NONE',  ( 5.178964085587577574E-17, 4.977861111186976828, 0.2819296736111110979 ) ) ;
#16953 = AXIS2_PLACEMENT_3D ( 'NONE', #17622, #15793, #10079 ) ;
#16954 = CARTESIAN_POINT ( 'NONE',  ( -0.1294417382415922191, 0.3125000000000000000, 0.001527777777779144386 ) ) ;
#16955 = SHAPE_REPRESENTATION ( 'Aloris-BXA-Handle-Rod', ( #9127 ), #14988 ) ;
#16956 = CARTESIAN_POINT ( 'NONE',  ( 0.08877758875623015244, 3.708028241517439927, -0.2996422185575408070 ) ) ;
#16957 = DIRECTION ( 'NONE',  ( -0.4999999999999916178, 0.000000000000000000, 0.8660254037844433705 ) ) ;
#16958 = CC_DESIGN_APPROVAL ( #14170, ( #4493 ) ) ;
#16959 = CARTESIAN_POINT ( 'NONE',  ( -0.2819296736111110979, 4.741750000075865223, 0.000000000000000000 ) ) ;
#16960 = ITEM_DEFINED_TRANSFORMATION ( 'NONE', 'NONE', #13840,  #9127 ) ;
#16961 = CARTESIAN_POINT ( 'NONE',  ( 0.3119999999999999996, 4.300777777777777366, -3.820898013339742174E-17 ) ) ;
#16962 = DIRECTION ( 'NONE',  ( -0.000000000000000000, 1.000000000000000000, -0.000000000000000000 ) ) ;
#16963 = CARTESIAN_POINT ( 'NONE',  ( 0.2819296736111110979, 0.4381944443685778512, 0.000000000000000000 ) ) ;
#16964 = ORIENTED_EDGE ( 'NONE', *, *, #20049, .F. ) ;
#16965 = CARTESIAN_POINT ( 'NONE',  ( -0.1993543840281267465, 0.1951388888130222710, 0.1993543840281266633 ) ) ;
#16966 = CARTESIAN_POINT ( 'NONE',  ( 0.000000000000000000, 3.700000000000000622, 0.000000000000000000 ) ) ;
#16967 = CARTESIAN_POINT ( 'NONE',  ( -0.2082794372640225100, 5.206640035683668621, 0.1900105704308308607 ) ) ;
#16968 = CARTESIAN_POINT ( 'NONE',  ( -0.3236067977499790249, 0.2285714285714285088, 0.2351141009169892271 ) ) ;
#16969 = CARTESIAN_POINT ( 'NONE',  ( -0.1306872919485615459, -0.3155070326520293400, 0.2393750000000029465 ) ) ;
#16970 = CARTESIAN_POINT ( 'NONE',  ( -0.2726274893998237858, -0.3838643229717944583, 0.09139053646026255862 ) ) ;
#16971 = LINE ( 'NONE', #10270, #5462 ) ;
#16972 = CARTESIAN_POINT ( 'NONE',  ( -5.178964085587577574E-17, 0.2993055554796889561, 0.2819296736111110979 ) ) ;
#16973 = CARTESIAN_POINT ( 'NONE',  ( -0.1167790944451422702, 0.2194444443685777957, -0.2819296736111110424 ) ) ;
#16974 = CARTESIAN_POINT ( 'NONE',  ( -0.2819296736111110424, 4.259111111186976828, 0.1167790944451424923 ) ) ;
#16975 = CARTESIAN_POINT ( 'NONE',  ( -0.3236067977499789694, 0.06249999980491521834, -0.2351141009169893104 ) ) ;
#16976 = EDGE_CURVE ( 'NONE', #9142, #9842, #580, .T. ) ;
#16977 = CARTESIAN_POINT ( 'NONE',  ( 0.1167790944451422702, 4.904944444520311642, -0.2819296736111110424 ) ) ;
#16978 = EDGE_CURVE ( 'NONE', #16899, #4071, #6626, .T. ) ;
#16979 = CARTESIAN_POINT ( 'NONE',  ( -1.726321361862525858E-17, 4.505638888964754507, -0.2819296736111110979 ) ) ;
#16980 = FACE_OUTER_BOUND ( 'NONE', #15639, .T. ) ;
#16981 = SECURITY_CLASSIFICATION ( '', '', #23183 ) ;
#16982 = PERSON ( 'NAUO-PER6', 'UNSPECIFIED', 'UNSPECIFIED', ('UNSPECIFIED'), ('UNSPECIFIED'), ('UNSPECIFIED') ) ;
#16983 = VERTEX_POINT ( 'NONE', #6874 ) ;
#16984 = DIRECTION ( 'NONE',  ( -0.000000000000000000, -1.000000000000000000, -0.000000000000000000 ) ) ;
#16985 = CARTESIAN_POINT ( 'NONE',  ( -0.2206173157302028232, 4.106333333485065573, -0.2206173157302028232 ) ) ;
#16986 = CARTESIAN_POINT ( 'NONE',  ( 0.3950000000000000178, 0.05000000000000028727, -1.966000000000000192 ) ) ;
#16987 = CARTESIAN_POINT ( 'NONE',  ( -0.3866234456863465452, 2.661589509557314770, 2.621538993229147962 ) ) ;
#16988 = ORIENTED_EDGE ( 'NONE', *, *, #12930, .T. ) ;
#16989 = PERSON_AND_ORGANIZATION ( #15518, #2538 ) ;
#16990 = EDGE_LOOP ( 'NONE', ( #8421, #11754, #6736, #7917, #9398 ) ) ;
#16991 = DIRECTION ( 'NONE',  ( 0.000000000000000000, 0.7071067811865497932, 0.7071067811865452413 ) ) ;
#16992 = CARTESIAN_POINT ( 'NONE',  ( -0.3616234456863258173, 4.559812086079793048, -2.727383698113316157 ) ) ;
#16993 = ORIENTED_EDGE ( 'NONE', *, *, #21301, .T. ) ;
#16994 = CARTESIAN_POINT ( 'NONE',  ( -0.2206173157302028787, 0.5458333331816004330, 0.2206173157302027954 ) ) ;
#16995 = ORIENTED_EDGE ( 'NONE', *, *, #4532, .T. ) ;
#16996 = DIRECTION ( 'NONE',  ( -0.000000000000000000, -1.000000000000000000, -0.000000000000000000 ) ) ;
#16997 = CARTESIAN_POINT ( 'NONE',  ( 0.000000000000000000, 5.384999999999999787, -0.3119999999999999996 ) ) ;
#16998 = CARTESIAN_POINT ( 'NONE',  ( 0.001301388441426008921, 4.766018610250637444, -0.3119976773732344166 ) ) ;
#16999 = CARTESIAN_POINT ( 'NONE',  ( 2.326421213736078119E-17, -0.05982142866897093708, -0.3799334167787516425 ) ) ;
#17000 = CARTESIAN_POINT ( 'NONE',  ( 0.04081095154783396378, 3.961648846695317250, 0.3119999993940247851 ) ) ;
#17001 = ORIENTED_EDGE ( 'NONE', *, *, #2306, .F. ) ;
#17002 = CARTESIAN_POINT ( 'NONE',  ( 0.2923287055106771337, 0.2187499999024575537, 0.2123892367102621359 ) ) ;
#17003 = AXIS2_PLACEMENT_3D ( 'NONE', #11452, #5948, #2303 ) ;
#17004 = EDGE_LOOP ( 'NONE', ( #17869, #2595, #22533, #15194, #8618, #20824 ) ) ;
#17005 = DIRECTION ( 'NONE',  ( 0.000000000000000000, 0.000000000000000000, 1.000000000000000000 ) ) ;
#17006 = CARTESIAN_POINT ( 'NONE',  ( 0.000000000000000000, 0.2764156081756484196, 0.4633333333333382043 ) ) ;
#17007 = CARTESIAN_POINT ( 'NONE',  ( -0.2819296736111110979, 3.963972222298087544, 0.000000000000000000 ) ) ;
#17008 = CARTESIAN_POINT ( 'NONE',  ( 0.1857303984225210092, 5.038301444411008134, -0.2517477023668195923 ) ) ;
#17009 = CARTESIAN_POINT ( 'NONE',  ( -4.974594353761572974E-07, 4.738258141874186258, 0.3119999999991586170 ) ) ;
#17010 = CARTESIAN_POINT ( 'NONE',  ( -0.2206173157302027676, 3.779944444444443441, 0.2206173157302028787 ) ) ;
#17011 = CARTESIAN_POINT ( 'NONE',  ( -1.910449006669871087E-17, 4.821611111262843252, -0.3119999999999999996 ) ) ;
#17012 = CARTESIAN_POINT ( 'NONE',  ( 0.2819296736111111534, 4.891055555631421470, 0.1167790944451422563 ) ) ;
#17013 = ORIENTED_EDGE ( 'NONE', *, *, #14991, .T. ) ;
#17014 = CARTESIAN_POINT ( 'NONE',  ( 0.1993543840281266633, 4.220916666742532186, -0.1993543840281266910 ) ) ;
#17015 = CARTESIAN_POINT ( 'NONE',  ( -0.2568804798144080914, 3.896411533234364732, 0.1790538691666017646 ) ) ;
#17016 = VERTEX_POINT ( 'NONE', #16145 ) ;
#17017 = CARTESIAN_POINT ( 'NONE',  ( 0.1116596296178199027, 0.05089285704531473081, 0.3436530038418508792 ) ) ;
#17018 = VERTEX_POINT ( 'NONE', #14317 ) ;
#17019 = VECTOR ( 'NONE', #1847, 39.37007874015748854 ) ;
#17020 = EDGE_LOOP ( 'NONE', ( #9676, #4566, #16249, #15665, #14006 ) ) ;
#17021 = PERSON_AND_ORGANIZATION ( #15518, #2538 ) ;
#17022 = CARTESIAN_POINT ( 'NONE',  ( 0.000000000000000000, 0.3155070326520292845, 0.4407638888888937845 ) ) ;
#17023 = CARTESIAN_POINT ( 'NONE',  ( -0.2819296736111110424, 5.182722222298088433, -0.1167790944451423119 ) ) ;
#17024 = CARTESIAN_POINT ( 'NONE',  ( 5.178964085587577574E-17, 3.825083333409199149, 0.2819296736111110979 ) ) ;
#17025 = DIRECTION ( 'NONE',  ( -0.4985709748471497393, -0.07555085810113111588, 0.8635502596144276621 ) ) ;
#17026 = ADVANCED_FACE ( 'NONE', ( #12259 ), #21388, .T. ) ;
#17027 = CARTESIAN_POINT ( 'NONE',  ( -0.4453125000000000000, -5.453505277453057578E-17, 0.4425000000000000044 ) ) ;
#17028 = ORIENTED_EDGE ( 'NONE', *, *, #18851, .T. ) ;
#17029 = CARTESIAN_POINT ( 'NONE',  ( 0.1954553509668046640, -0.1954553509668047195, 0.3313888888888926743 ) ) ;
#17030 = CARTESIAN_POINT ( 'NONE',  ( 0.2819296736111110979, 0.6048611110352445364, 0.000000000000000000 ) ) ;
#17031 = CARTESIAN_POINT ( 'NONE',  ( 0.1954553509668046640, -0.1954553509668047195, -0.1130555555555552844 ) ) ;
#17032 = CARTESIAN_POINT ( 'NONE',  ( 0.2819296736111110979, 5.057722222298088433, 0.1167790944451422425 ) ) ;
#17033 = CARTESIAN_POINT ( 'NONE',  ( -9.626299801968715084E-16, 0.4089285712334866374, -0.4000000000000000222 ) ) ;
#17034 = CARTESIAN_POINT ( 'NONE',  ( -0.2819296736111110979, 4.686194444520309865, 0.000000000000000000 ) ) ;
#17035 = CARTESIAN_POINT ( 'NONE',  ( -0.2663171304906524761, 0.09313777201924451632, -0.07114126500001324849 ) ) ;
#17036 = CARTESIAN_POINT ( 'NONE',  ( 0.1059882155383018582, 4.852523979370922724, 0.2940631531866885195 ) ) ;
#17037 = CARTESIAN_POINT ( 'NONE',  ( 0.5800849365154925330, 2.740000000000000213, -0.6888427490622308635 ) ) ;
#17038 = DIRECTION ( 'NONE',  ( -0.000000000000000000, -1.000000000000000000, -0.000000000000000000 ) ) ;
#17039 = CARTESIAN_POINT ( 'NONE',  ( 0.3119999999999999996, 4.575083333333332725, 0.1292346314604056190 ) ) ;
#17040 = VECTOR ( 'NONE', #14367, 39.37007874015748143 ) ;
#17041 = CARTESIAN_POINT ( 'NONE',  ( 0.1167790944451424506, 3.870222222298087988, 0.2819296736111110424 ) ) ;
#17042 = CARTESIAN_POINT ( 'NONE',  ( 0.09330201573823466987, 4.985571540157835102, -0.2986323972303005503 ) ) ;
#17043 = B_SPLINE_CURVE_WITH_KNOTS ( 'NONE', 3,
 ( #7937, #22583, #22699, #8061, #15153, #386, #15391, #5759 ),
 .UNSPECIFIED., .F., .F.,
 ( 4, 2, 2, 4 ),
 ( 0.000000000000000000, 0.002297969625092518512, 0.003446954437638777985, 0.004595939250185037024 ),
 .UNSPECIFIED. ) ;
#17044 = ORIENTED_EDGE ( 'NONE', *, *, #16802, .T. ) ;
#17045 = PLANE ( 'NONE',  #15557 ) ;
#17046 = VERTEX_POINT ( 'NONE', #6388 ) ;
#17047 = CARTESIAN_POINT ( 'NONE',  ( 0.4687500000000002776, -0.2598076211353317344, 0.06112444011295376650 ) ) ;
#17048 = EDGE_CURVE ( 'NONE', #14200, #15698, #19674, .T. ) ;
#17049 = CARTESIAN_POINT ( 'NONE',  ( 0.2131833129333350341, 4.648326027883385336, -0.2316251136011019396 ) ) ;
#17050 = CARTESIAN_POINT ( 'NONE',  ( 0.1144950937579611444, 0.2764156081756483641, 0.4043055555555599145 ) ) ;
#17051 = CIRCLE ( 'NONE', #8078, 0.03500000000000003803 ) ;
#17052 = CARTESIAN_POINT ( 'NONE',  ( -5.428794840643969700E-10, 4.321611111277808170, -0.3119999999999999996 ) ) ;
#17053 = EDGE_CURVE ( 'NONE', #12392, #789, #17352, .T. ) ;
#17054 = CARTESIAN_POINT ( 'NONE',  ( 0.2934357671952408375, 5.143311997241705846, 0.08181467001294073782 ) ) ;
#17055 = ORIENTED_EDGE ( 'NONE', *, *, #14379, .F. ) ;
#17056 = CARTESIAN_POINT ( 'NONE',  ( 0.3613381517857143232, 0.06874999990245758696, -0.1174058825155740587 ) ) ;
#17057 = CARTESIAN_POINT ( 'NONE',  ( 0.1167790944451423535, 0.5805555554796888451, 0.2819296736111110424 ) ) ;
#17058 = DIRECTION ( 'NONE',  ( 1.707404996040164512E-16, 0.000000000000000000, -1.000000000000000000 ) ) ;
#17059 = CARTESIAN_POINT ( 'NONE',  ( 0.1236067977499789861, 0.04821428551920090705, -0.3804226065180614236 ) ) ;
#17060 = LINE ( 'NONE', #5483, #1963 ) ;
#17061 = CARTESIAN_POINT ( 'NONE',  ( 0.2764156081756483641, -0.1144950937579611167, 0.2862500000000034461 ) ) ;
#17062 = LINE ( 'NONE', #9508, #3652 ) ;
#17063 = CARTESIAN_POINT ( 'NONE',  ( -0.5116234456863258950, 4.559812086079788607, -2.640781157734871876 ) ) ;
#17064 = CARTESIAN_POINT ( 'NONE',  ( 0.1292346314604057023, 0.1743055555555551861, 0.3119999999999998885 ) ) ;
#17065 = CARTESIAN_POINT ( 'NONE',  ( 5.731347020009612645E-17, 5.120222222222221120, 0.3119999999999999996 ) ) ;
#17066 = CARTESIAN_POINT ( 'NONE',  ( -0.2819296736111110424, 4.259111111186976828, 0.1167790944451424923 ) ) ;
#17067 = CARTESIAN_POINT ( 'NONE',  ( -0.1570450868762801044, 4.344718169250874062, 0.2726662231104447498 ) ) ;
#17068 = ADVANCED_FACE ( 'NONE', ( #20286 ), #5525, .T. ) ;
#17069 = CARTESIAN_POINT ( 'NONE',  ( 0.000000000000000000, 5.384999999999999787, 0.000000000000000000 ) ) ;
#17070 = EDGE_LOOP ( 'NONE', ( #9168, #18101 ) ) ;
#17071 = ORIENTED_EDGE ( 'NONE', *, *, #7661, .F. ) ;
#17072 = VECTOR ( 'NONE', #14821, 39.37007874015748143 ) ;
#17073 = CARTESIAN_POINT ( 'NONE',  ( 0.3065849364905491314, 4.945545817829770315E-15, 0.4182516031572158233 ) ) ;
#17074 = CARTESIAN_POINT ( 'NONE',  ( 0.1167790944451422702, 5.057722222298087544, -0.2819296736111110424 ) ) ;
#17075 = CARTESIAN_POINT ( 'NONE',  ( 0.2026594160797257904, -0.4367605021652135600, 0.07441357458167795202 ) ) ;
#17076 = EDGE_CURVE ( 'NONE', #15412, #10865, #23168, .T. ) ;
#17077 = CARTESIAN_POINT ( 'NONE',  ( -0.3003886044924828358, 5.154938911184799188, -0.02224241330659365926 ) ) ;
#17078 = ADVANCED_FACE ( 'NONE', ( #10787 ), #13463, .T. ) ;
#17079 = ADVANCED_FACE ( 'NONE', ( #19170 ), #3612, .F. ) ;
#17080 = CARTESIAN_POINT ( 'NONE',  ( 1.573500000000000343, -0.07548905652294785051, -1.412499999999999645 ) ) ;
#17081 = CARTESIAN_POINT ( 'NONE',  ( 0.4800179196285669914, -0.1716494391952127496, 0.06108892084617357360 ) ) ;
#17082 = CARTESIAN_POINT ( 'NONE',  ( -0.1954553509668046918, -0.1954553509668046640, -0.1269444444444442766 ) ) ;
#17083 = CARTESIAN_POINT ( 'NONE',  ( 0.2819296736111110979, 4.283416666742533074, -3.452642723725051716E-17 ) ) ;
#17084 = SECURITY_CLASSIFICATION_LEVEL ( 'unclassified' ) ;
#17085 = ADVANCED_FACE ( 'NONE', ( #16980 ), #20998, .T. ) ;
#17086 = CARTESIAN_POINT ( 'NONE',  ( 1.910449006669871087E-17, 0.6361111109593781121, -0.3119999999999999996 ) ) ;
#17087 = MANIFOLD_SOLID_BREP ( '1/2-13 Tapped Hole', #1412 ) ;
#17088 = CARTESIAN_POINT ( 'NONE',  ( 0.2764156081756483641, 0.1144950937579610195, -0.04013888888888804407 ) ) ;
#17089 = B_SPLINE_CURVE_WITH_KNOTS ( 'NONE', 3,
 ( #19676, #23562, #12505, #10433, #12386, #6877, #19802, #8455, #19926, #10659, #3213, #8822, #7002, #5160, #17611, #901, #6513, #13961, #12261, #21391, #4680, #12150, #19556, #1024, #15898, #6628, #154, #21988, #14691 ),
 .UNSPECIFIED., .F., .F.,
 ( 4, 2, 1, 1, 1, 2, 2, 2, 2, 2, 2, 2, 2, 2, 2, 4 ),
 ( 0.2837225594813787555, 0.2840009242586815086, 0.2841401066473329129, 0.2842096978416585595, 0.2842444934388214106, 0.2842618912374028639, 0.2842792890359842617, 0.2848360185905898234, 0.2859494776998008359, 0.2881763959182229717, 0.2904033141366450521, 0.2926302323550671880, 0.2948571505734892684, 0.2970840687919114043, 0.2993109870103335401, 0.3015379052287556205 ),
 .UNSPECIFIED. ) ;
#17090 = CARTESIAN_POINT ( 'NONE',  ( -0.2819296736111110979, 0.5215277777019110550, -3.452642723725051716E-17 ) ) ;
#17092 = ORIENTED_EDGE ( 'NONE', *, *, #21035, .T. ) ;
#17091 = CIRCLE ( 'NONE', #6571, 0.6398935782932173577 ) ;
#17093 = CARTESIAN_POINT ( 'NONE',  ( 0.2819296736111110424, 0.5527777777019111660, -0.1167790944451423119 ) ) ;
#17094 = CARTESIAN_POINT ( 'NONE',  ( 5.731347020009612645E-17, 4.120222222222221120, 0.3119999999999999996 ) ) ;
#17095 = DIRECTION ( 'NONE',  ( -1.000000000000000000, 0.000000000000000000, 0.000000000000000000 ) ) ;
#17096 = CARTESIAN_POINT ( 'NONE',  ( -0.1236067977499790416, 0.1642857142857142294, 0.3804226065180614236 ) ) ;
#17097 = CARTESIAN_POINT ( 'NONE',  ( -0.3155070326520293400, 0.1306872919485614903, 0.2254861111111138572 ) ) ;
#17098 = CARTESIAN_POINT ( 'NONE',  ( 0.4687500000000003886, 0.04344991094760242145, 0.4181619485698828131 ) ) ;
#17099 = DIRECTION ( 'NONE',  ( 0.8660254037844434816, 0.000000000000000000, -0.4999999999999914513 ) ) ;
#17100 = CARTESIAN_POINT ( 'NONE',  ( 0.1167790944451423535, 0.5805555554796890672, 0.2819296736111110979 ) ) ;
#17101 = CARTESIAN_POINT ( 'NONE',  ( -0.2819296736111110424, 0.1152777777019111521, -0.1167790944451423396 ) ) ;
#17102 = CARTESIAN_POINT ( 'NONE',  ( 0.1167790944451422702, 4.349388888964754507, -0.2819296736111110424 ) ) ;
#17103 = CARTESIAN_POINT ( 'NONE',  ( -0.1236067977499789583, 0.4124999998049151406, -0.3804226065180614791 ) ) ;
#17104 = CARTESIAN_POINT ( 'NONE',  ( 0.1167790944451422702, 4.960500000075865223, -0.2819296736111110424 ) ) ;
#17105 = CARTESIAN_POINT ( 'NONE',  ( -1.726321361862525858E-17, 4.450083333409198261, -0.2819296736111110979 ) ) ;
#17106 = CARTESIAN_POINT ( 'NONE',  ( 0.03174294256098300626, 2.685901063997346405, -0.8524985337548631747 ) ) ;
#17107 = VERTEX_POINT ( 'NONE', #7944 ) ;
#17108 = CARTESIAN_POINT ( 'NONE',  ( -1.910449006669871087E-17, 4.536888888888888083, -0.3119999999999999996 ) ) ;
#17109 = CARTESIAN_POINT ( 'NONE',  ( 0.3119999999999999996, 4.026472222373954857, 0.1292346314604056190 ) ) ;
#17110 =( BOUNDED_CURVE ( )  B_SPLINE_CURVE ( 2, ( #7530, #20458, #11197, #10959, #18384, #14615, #22160, #12800, #3385 ),
 .UNSPECIFIED., .F., .T. ) 
 B_SPLINE_CURVE_WITH_KNOTS ( ( 3, 2, 2, 2, 3 ),
 ( 0.4375000000000000555, 0.4419642857142857539, 0.4464285714285715079, 0.4508928571428572618, 0.4553571428571429602 ),
 .UNSPECIFIED. ) 
 CURVE ( )  GEOMETRIC_REPRESENTATION_ITEM ( )  RATIONAL_B_SPLINE_CURVE ( ( 0.9999999999999990008, 0.9238795325112877377, 1.000000000000000000, 0.9238795325112867385, 1.000000000000000000, 0.9238795325112867385, 1.000000000000000000, 0.9238795325112848511, 1.000000000000001998 ) ) 
 REPRESENTATION_ITEM ( '' )  );
#17111 = VECTOR ( 'NONE', #12168, 39.37007874015748143 ) ;
#17112 = CARTESIAN_POINT ( 'NONE',  ( 0.08700723303891660931, -0.2927098606305870709, -0.09407488447002992915 ) ) ;
#17113 = ORIENTED_EDGE ( 'NONE', *, *, #21094, .T. ) ;
#17114 = EDGE_CURVE ( 'NONE', #11818, #9048, #6239, .T. ) ;
#17115 = APPROVAL_STATUS ( 'not_yet_approved' ) ;
#17116 = VERTEX_POINT ( 'NONE', #15517 ) ;
#17117 = EDGE_CURVE ( 'NONE', #13298, #17016, #9669, .T. ) ;
#17118 = CARTESIAN_POINT ( 'NONE',  ( 0.1038682246014075439, 0.2678606782618273008, 0.3984990337825972673 ) ) ;
#17119 = CARTESIAN_POINT ( 'NONE',  ( 0.7948333950160438865, 2.675000000000000711, -3.001000000000001666 ) ) ;
#17120 = CARTESIAN_POINT ( 'NONE',  ( -0.5116234456863258950, 4.559812086079793048, -2.640781157734872320 ) ) ;
#17121 = ORIENTED_EDGE ( 'NONE', *, *, #15666, .T. ) ;
#17122 = CARTESIAN_POINT ( 'NONE',  ( 0.3119999999999999996, 0.3999999998482670627, 0.000000000000000000 ) ) ;
#17123 = ORIENTED_EDGE ( 'NONE', *, *, #18094, .T. ) ;
#17124 = CARTESIAN_POINT ( 'NONE',  ( 0.3119648635814757931, 4.250952432720125351, 0.04117389441842130016 ) ) ;
#17125 = CARTESIAN_POINT ( 'NONE',  ( 0.000000000000000000, 0.7650000000000000133, 0.000000000000000000 ) ) ;
#17126 = CARTESIAN_POINT ( 'NONE',  ( 1.910449006669871087E-17, 0.5319444444444439979, -0.3119999999999999996 ) ) ;
#17127 = CARTESIAN_POINT ( 'NONE',  ( 0.1116596296178199860, 0.008035714188171883682, -0.3436530038418508792 ) ) ;
#17128 = CARTESIAN_POINT ( 'NONE',  ( 0.09437171819121717431, 5.169739643388256312, 0.2818761894294421477 ) ) ;
#17129 = ORIENTED_EDGE ( 'NONE', *, *, #7635, .T. ) ;
#17130 = CARTESIAN_POINT ( 'NONE',  ( 0.1116596296178199860, 0.3116071427596003862, -0.3436530038418508792 ) ) ;
#17131 = CIRCLE ( 'NONE', #7398, 1.048989065017511546 ) ;
#17132 = ORIENTED_EDGE ( 'NONE', *, *, #11663, .T. ) ;
#17133 = CARTESIAN_POINT ( 'NONE',  ( 0.8977114317029943891, 2.291712385858714729, -0.6297771125693037986 ) ) ;
#17134 = CARTESIAN_POINT ( 'NONE',  ( -0.2764156081756484196, 1.692557448933383907E-17, 0.4216666666666711860 ) ) ;
#17135 = CARTESIAN_POINT ( 'NONE',  ( 0.2819296736111110979, 4.099388888964754507, 0.1167790944451422425 ) ) ;
#17136 = CARTESIAN_POINT ( 'NONE',  ( 0.000000000000000000, 3.659999999999999698, 0.000000000000000000 ) ) ;
#17137 = LINE ( 'NONE', #5674, #3816 ) ;
#17138 = CARTESIAN_POINT ( 'NONE',  ( 0.000000000000000000, 5.579732050807569621, -0.2499999999999999722 ) ) ;
#17139 = CARTESIAN_POINT ( 'NONE',  ( -0.2206173157302028232, 4.717444444596176290, -0.2206173157302028232 ) ) ;
#17140 = CARTESIAN_POINT ( 'NONE',  ( -0.1993543840281266910, 5.026472222298088433, -0.1993543840281266910 ) ) ;
#17141 = ORIENTED_EDGE ( 'NONE', *, *, #1301, .F. ) ;
#17142 = CARTESIAN_POINT ( 'NONE',  ( -0.1993543840281266355, 4.304250000075865223, 0.1993543840281267465 ) ) ;
#17143 = EDGE_LOOP ( 'NONE', ( #24031, #19486, #18794, #5319 ) ) ;
#17144 = AXIS2_PLACEMENT_3D ( 'NONE', #19788, #16376, #19664 ) ;
#17145 = AXIS2_PLACEMENT_3D ( 'NONE', #22500, #13021, #18608 ) ;
#17146 = VERTEX_POINT ( 'NONE', #512 ) ;
#17147 = COORDINATED_UNIVERSAL_TIME_OFFSET ( 0, 0, .AHEAD. ) ;
#17148 = PLANE ( 'NONE',  #11478 ) ;
#17149 = DIRECTION ( 'NONE',  ( 0.000000000000000000, 1.000000000000000000, 0.000000000000000000 ) ) ;
#17150 = CARTESIAN_POINT ( 'NONE',  ( -0.1167790944451423535, 3.877166666742532186, 0.2819296736111110979 ) ) ;
#17151 = FACE_OUTER_BOUND ( 'NONE', #1996, .T. ) ;
#17152 = CARTESIAN_POINT ( 'NONE',  ( -1.910449006669871087E-17, 4.647999999999998799, -0.3119999999999999996 ) ) ;
#17153 = CARTESIAN_POINT ( 'NONE',  ( 0.08492194567809631389, -0.4922361691679447704, 0.06591465713334185295 ) ) ;
#17154 = CARTESIAN_POINT ( 'NONE',  ( 0.2764156081756484196, -5.077672346800151106E-17, 0.2827777777777812362 ) ) ;
#17155 = CARTESIAN_POINT ( 'NONE',  ( -0.1993543840281266633, 0.4590277777019111105, -0.1993543840281266910 ) ) ;
#17156 = CARTESIAN_POINT ( 'NONE',  ( -3.385114897866767815E-17, -0.2764156081756484196, -0.1199999999999997735 ) ) ;
#17157 = VERTEX_POINT ( 'NONE', #5878 ) ;
#17158 = CARTESIAN_POINT ( 'NONE',  ( -0.1167790944451423535, 4.766055555631421470, 0.2819296736111110424 ) ) ;
#17159 = CARTESIAN_POINT ( 'NONE',  ( 0.01172578639831967605, -0.5344959914317446437, 0.04874733047933996199 ) ) ;
#17160 = CARTESIAN_POINT ( 'NONE',  ( 0.1993543840281267465, 4.595916666742532186, 0.1993543840281266633 ) ) ;
#17161 = CARTESIAN_POINT ( 'NONE',  ( -0.1695524133009077561, 0.2302630372892206234, -0.07448633787354336233 ) ) ;
#17162 = CIRCLE ( 'NONE', #6238, 0.3253415854805813412 ) ;
#17163 = EDGE_CURVE ( 'NONE', #7263, #23447, #22828, .T. ) ;
#17164 = CARTESIAN_POINT ( 'NONE',  ( 0.2093153376853872927, 4.855910065012234433, 0.2313697181335848119 ) ) ;
#17165 = CARTESIAN_POINT ( 'NONE',  ( 1.457716030923678074, 2.291712385858714729, -2.174029041877829194 ) ) ;
#17166 = CYLINDRICAL_SURFACE ( 'NONE', #9644, 0.3119999999999999996 ) ;
#17167 = CARTESIAN_POINT ( 'NONE',  ( -0.2206173157302027676, 4.502166666666665762, 0.2206173157302028787 ) ) ;
#17168 = AXIS2_PLACEMENT_3D ( 'NONE', #22094, #16378, #14306 ) ;
#17169 = EDGE_CURVE ( 'NONE', #15406, #2181, #22310, .T. ) ;
#17170 = CARTESIAN_POINT ( 'NONE',  ( -0.1993543840281266355, 3.804250000075865223, 0.1993543840281267465 ) ) ;
#17171 = CARTESIAN_POINT ( 'NONE',  ( -0.06335377612981410445, 0.2374552042304697019, 0.4000000000000001887 ) ) ;
#17172 = VERTEX_POINT ( 'NONE', #6117 ) ;
#17173 = CARTESIAN_POINT ( 'NONE',  ( 0.000000000000000000, 5.384999999999999787, 0.000000000000000000 ) ) ;
#17174 = ORIENTED_EDGE ( 'NONE', *, *, #2660, .T. ) ;
#17175 = PRODUCT_RELATED_PRODUCT_CATEGORY ( 'detail', '', ( #19837 ) ) ;
#17176 = EDGE_CURVE ( 'NONE', #1317, #22119, #5423, .T. ) ;
#17177 = CARTESIAN_POINT ( 'NONE',  ( 0.2206238289344933934, 4.703650875443257107, -0.2218057234084611085 ) ) ;
#17178 = CARTESIAN_POINT ( 'NONE',  ( 0.1144950937579609085, -0.2764156081756484751, 0.3834722222222265442 ) ) ;
#17179 = VECTOR ( 'NONE', #18573, 39.37007874015748143 ) ;
#17180 = CYLINDRICAL_SURFACE ( 'NONE', #4480, 0.3125000000000000000 ) ;
#17181 = ORIENTED_EDGE ( 'NONE', *, *, #11553, .F. ) ;
#17182 = CARTESIAN_POINT ( 'NONE',  ( 0.2923287055106771337, 0.4330357141881717720, 0.2123892367102621359 ) ) ;
#17183 = CARTESIAN_POINT ( 'NONE',  ( 0.2819296736111110424, 0.5388888888130223265, -0.1167790944451423119 ) ) ;
#17184 = CARTESIAN_POINT ( 'NONE',  ( -0.1802044324038121481, 5.206640035683668621, 0.2176895457663558520 ) ) ;
#17185 = CARTESIAN_POINT ( 'NONE',  ( 0.2375040497016436547, 0.2775713580457571661, -1.193554297574972001 ) ) ;
#17186 = LINE ( 'NONE', #16828, #3913 ) ;
#17187 = CARTESIAN_POINT ( 'NONE',  ( -0.1954553509668046640, 0.1954553509668046918, 0.1994444444444471720 ) ) ;
#17188 = CARTESIAN_POINT ( 'NONE',  ( -0.1858657769656070491, 4.621489086676496605, 0.2509059806342907595 ) ) ;
#17189 = CARTESIAN_POINT ( 'NONE',  ( -1.910449006669871087E-17, 4.370222222222221120, -0.3119999999999999996 ) ) ;
#17190 = CARTESIAN_POINT ( 'NONE',  ( -0.05636693431585264313, -3.088309080874367638E-17, -0.3805424261366754934 ) ) ;
#17191 = CARTESIAN_POINT ( 'NONE',  ( -0.3119999999999999996, 0.3201388888888885287, -0.1292346314604056745 ) ) ;
#17192 = CARTESIAN_POINT ( 'NONE',  ( -0.3119999999999998885, 5.109805555555555046, 0.1292346314604058410 ) ) ;
#17193 = B_SPLINE_CURVE_WITH_KNOTS ( 'NONE', 3,
 ( #22902, #6078, #10354, #15826, #19368, #13544, #11704, #17300, #17421, #19127, #945, #593, #834, #17658, #21077, #15712, #8375, #23245, #8025, #11824, #19244, #23016 ),
 .UNSPECIFIED., .F., .F.,
 ( 4, 2, 2, 2, 2, 2, 2, 2, 2, 2, 4 ),
 ( 0.002245614500286350051, 0.002912534838771771700, 0.003579455177257192915, 0.004913295854228036212, 0.006247136531198878642, 0.007580977208169723675, 0.008914817885140568707, 0.009581738223625988621, 0.01024865856211140853, 0.01158249923908224836, 0.01291633991605308993 ),
 .UNSPECIFIED. ) ;
#17194 = CARTESIAN_POINT ( 'NONE',  ( 0.1167790944451424368, 4.161888888964755395, 0.2819296736111110424 ) ) ;
#17195 = CARTESIAN_POINT ( 'NONE',  ( -0.5116234456863258950, 1.999640111863039582, -2.640781157734871876 ) ) ;
#17196 = CARTESIAN_POINT ( 'NONE',  ( 5.731347020009612645E-17, 3.786888888888888527, 0.3119999999999999996 ) ) ;
#17197 = CARTESIAN_POINT ( 'NONE',  ( 0.3308333333333332571, 3.738758431839877614E-19, 0.4425000000000000044 ) ) ;
#17198 = ORIENTED_EDGE ( 'NONE', *, *, #13082, .T. ) ;
#17199 = ORIENTED_EDGE ( 'NONE', *, *, #10536, .T. ) ;
#17200 = CARTESIAN_POINT ( 'NONE',  ( 0.2472135954999579721, 0.3303571426620581231, -0.3402603233408160732 ) ) ;
#17201 = CARTESIAN_POINT ( 'NONE',  ( -0.1167790944451423257, 4.786888888964755395, -0.2819296736111110424 ) ) ;
#17202 = EDGE_CURVE ( 'NONE', #11875, #13964, #18939, .T. ) ;
#17203 = CARTESIAN_POINT ( 'NONE',  ( -6.979263641208234666E-17, 0.4044642856167431910, 0.3799334167787516980 ) ) ;
#17204 = CARTESIAN_POINT ( 'NONE',  ( 0.2722827744214832979, -0.3840633442573331280, 0.4172182224143142770 ) ) ;
#17205 = DIRECTION ( 'NONE',  ( 0.009165238783119120797, 0.000000000000000000, 0.9999579983169535335 ) ) ;
#17206 = LINE ( 'NONE', #3794, #9194 ) ;
#17207 = CARTESIAN_POINT ( 'NONE',  ( -0.2764156081756484196, 1.692557448933383907E-17, -0.1338888888888887796 ) ) ;
#17208 = CARTESIAN_POINT ( 'NONE',  ( -0.1167790944451423535, 4.266055555631421470, 0.2819296736111110979 ) ) ;
#17209 = DATE_AND_TIME ( #9774, #3754 ) ;
#17210 = CARTESIAN_POINT ( 'NONE',  ( -0.1803192683449008904, 4.049281307906420047, -0.2549174622237436738 ) ) ;
#17211 = CARTESIAN_POINT ( 'NONE',  ( -0.2195630361087207438, -0.1679215936615484073, -0.06558227484231504700 ) ) ;
#17212 = VERTEX_POINT ( 'NONE', #395 ) ;
#17213 = CARTESIAN_POINT ( 'NONE',  ( 0.1167790944451423535, 0.3722222221463555858, 0.2819296736111110424 ) ) ;
#17214 = DIRECTION ( 'NONE',  ( -0.000000000000000000, -1.000000000000000000, -0.000000000000000000 ) ) ;
#17215 = CARTESIAN_POINT ( 'NONE',  ( -0.2427785569044363101, 5.205301948546705582, 0.1471746161278502940 ) ) ;
#17216 = CARTESIAN_POINT ( 'NONE',  ( 0.2472135954999579721, 0.1249999999999999306, -0.3402603233408159622 ) ) ;
#17217 = CARTESIAN_POINT ( 'NONE',  ( 0.2230971623002953874, -0.2230971623002954429, 0.1942361111111136074 ) ) ;
#17218 = FACE_OUTER_BOUND ( 'NONE', #15080, .T. ) ;
#17219 = EDGE_CURVE ( 'NONE', #17018, #13133, #15279, .T. ) ;
#17220 = CARTESIAN_POINT ( 'NONE',  ( 0.000000000000000000, 0.000000000000000000, -0.1012499999999999928 ) ) ;
#17221 = CARTESIAN_POINT ( 'NONE',  ( 0.1993543840281266910, 0.4312499999241333759, -0.1993543840281266910 ) ) ;
#17222 = CARTESIAN_POINT ( 'NONE',  ( -0.2819296736111110979, 0.1187499999241333620, -3.452642723725051716E-17 ) ) ;
#17223 = EDGE_LOOP ( 'NONE', ( #16677, #16197, #11884, #12367 ) ) ;
#17224 = ADVANCED_FACE ( 'NONE', ( #22706 ), #636, .F. ) ;
#17225 = EDGE_CURVE ( 'NONE', #21966, #8012, #22467, .T. ) ;
#17226 = CARTESIAN_POINT ( 'NONE',  ( -1.726321361862525858E-17, 4.352861111186976828, -0.2819296736111110979 ) ) ;
#17227 = CARTESIAN_POINT ( 'NONE',  ( 0.2472135954999579721, 0.3303571426620581231, -0.3402603233408159622 ) ) ;
#17228 = CARTESIAN_POINT ( 'NONE',  ( -0.2819296736111110424, 4.863277777853643791, -0.1167790944451423119 ) ) ;
#17229 = CARTESIAN_POINT ( 'NONE',  ( -0.2819296736111110424, 4.189666666742533074, 0.1167790944451424923 ) ) ;
#17230 = DIRECTION ( 'NONE',  ( 0.000000000000000000, 0.000000000000000000, -1.000000000000000000 ) ) ;
#17231 = CARTESIAN_POINT ( 'NONE',  ( -0.3124999999999989453, -0.1294417382415932460, 0.2306944444444472830 ) ) ;
#17232 = CARTESIAN_POINT ( 'NONE',  ( -1.910449006669871087E-17, 3.766055555707287450, -0.3119999999999999996 ) ) ;
#17233 = ADVANCED_FACE ( 'NONE', ( #15160 ), #22593, .T. ) ;
#17234 = CARTESIAN_POINT ( 'NONE',  ( 0.000000000000000000, 0.1199999999999999678, -0.2109499999999995268 ) ) ;
#17235 = VERTEX_POINT ( 'NONE', #9547 ) ;
#17236 = SHAPE_DEFINITION_REPRESENTATION ( #14604, #16955 ) ;
#17237 = AXIS2_PLACEMENT_3D ( 'NONE', #8507, #16317, #14010 ) ;
#17238 = CARTESIAN_POINT ( 'NONE',  ( 0.2799731695447734148, 0.01905728454626108223, 0.3921285916995966847 ) ) ;
#17239 = CARTESIAN_POINT ( 'NONE',  ( -0.2284039324571512375, 5.008807737987557296, 0.2125498346988052012 ) ) ;
#17240 = ORIENTED_EDGE ( 'NONE', *, *, #22883, .F. ) ;
#17241 = B_SPLINE_CURVE_WITH_KNOTS ( 'NONE', 3,
 ( #98, #11208, #7425, #22536, #9617, #15228, #16573, #11450, #20707, #18635, #223, #16691 ),
 .UNSPECIFIED., .F., .F.,
 ( 4, 2, 2, 2, 2, 4 ),
 ( 0.000000000000000000, 0.003345931539952393900, 0.005018897309928591934, 0.006691863079904790401, 0.01003779461985718734, 0.01338372615980958427 ),
 .UNSPECIFIED. ) ;
#17242 = CARTESIAN_POINT ( 'NONE',  ( 0.1167790944451423257, 0.05972222214635558579, -0.2819296736111110424 ) ) ;
#17243 = ORIENTED_EDGE ( 'NONE', *, *, #6455, .F. ) ;
#17244 = CARTESIAN_POINT ( 'NONE',  ( 9.184850993605150903E-17, -3.937007874019685528E-05, -0.7500000000000001110 ) ) ;
#17245 = DIRECTION ( 'NONE',  ( 0.000000000000000000, 1.000000000000000000, 0.000000000000000000 ) ) ;
#17246 = CARTESIAN_POINT ( 'NONE',  ( -5.731347020009612645E-17, 0.5597222222222218990, 0.3119999999999999996 ) ) ;
#17247 = CARTESIAN_POINT ( 'NONE',  ( 0.2233192592356399997, 0.1473214284738861568, -0.3073725909049500049 ) ) ;
#17248 = CARTESIAN_POINT ( 'NONE',  ( 0.2930505947314048787, 5.179336701705883783, -0.01581200851164489551 ) ) ;
#17249 = ORIENTED_EDGE ( 'NONE', *, *, #4831, .T. ) ;
#17250 = CARTESIAN_POINT ( 'NONE',  ( -0.3613381517857143232, 0.2580357141881718386, -0.1174058825155741143 ) ) ;
#17251 = CARTESIAN_POINT ( 'NONE',  ( 0.000000000000000000, 5.500232050807569273, 0.000000000000000000 ) ) ;
#17252 = CARTESIAN_POINT ( 'NONE',  ( 0.000000000000000000, 0.2764156081756484196, 0.4077777777777822354 ) ) ;
#17253 = CARTESIAN_POINT ( 'NONE',  ( 5.178964085587577574E-17, 4.088972222298087544, 0.2819296736111110979 ) ) ;
#17254 =( BOUNDED_CURVE ( )  B_SPLINE_CURVE ( 2, ( #13862, #23220, #16048, #10450, #17876, #6651, #14216, #10326, #21652, #15802, #17752, #1168, #23101, #19456, #2639, #23461, #4583, #1291, #6529, #8607, #6410, #21290, #22986, #19342, #6291, #13744, #21169, #4458, #11922, #17508, #12043, #13981, #10206, #21409, #4698, #12165, #15038, #20516, #7023, #16737, #9539, #22461, #3932, #20631, #1414, #21890, #20397, #268, #7587, #3811, #4044, #8842, #11497, #7707, #2098, #19, #23582, #5869, #3232, #3688, #20753, #5517, #9297, #12980, #7467, #10683, #13331, #19946, #13220, #16289, #23702, #11375, #18932, #11257, #8717, #1983, #5638, #15154, #16972, #18564, #16859, #14466, #11135, #1853, #18117, #18803, #144, #16167, #6899, #22584, #5760, #14916, #22335, #13103, #18682, #9420, #14338, #21770, #5057, #12527, #15272, #21114, #17577, #8300, #6474, #7826, #4645, #19281, #2588, #6110, #13697, #13579, #12112, #6232, #17338, #13927, #17221, #15510, #21238, #22700, #867, #4528, #23164, #11740, #749, #11616, #8062, #387, #19162, #5990, #6357, #2469, #10034, #2230, #4404, #22936, #8177, #11867, #15752, #15631, #21357, #20872, #505, #17456, #13454, #4166, #7938, #23049, #20989, #4285, #9906, #13804, #11991, #631, #19403, #9790, #2701, #10153, #9662, #17100, #19048, #2350, #15392, #22820, #10746, #20006, #10507 ),
 .UNSPECIFIED., .F., .T. ) 
 B_SPLINE_CURVE_WITH_KNOTS ( ( 3, 2, 2, 2, 2, 2, 2, 2, 2, 2, 2, 2, 2, 2, 2, 2, 2, 2, 2, 2, 2, 2, 2, 2, 2, 2, 2, 2, 2, 2, 2, 2, 2, 2, 2, 2, 2, 2, 2, 2, 2, 2, 2, 2, 2, 2, 2, 2, 2, 2, 2, 2, 2, 2, 2, 2, 2, 2, 2, 2, 2, 2, 2, 2, 2, 2, 2, 2, 2, 2, 2, 2, 2, 2, 2, 2, 2, 2, 2, 2, 2, 2, 2, 3 ),
 ( 0.07882564326583262060, 0.08333333333333332871, 0.09375000000000000000, 0.1041666666666666713, 0.1145833333333333287, 0.1250000000000000000, 0.1354166666666666574, 0.1458333333333333426, 0.1562500000000000000, 0.1666666666666666574, 0.1770833333333333426, 0.1875000000000000000, 0.1979166666666666574, 0.2083333333333333703, 0.2187500000000000000, 0.2291666666666666852, 0.2395833333333333703, 0.2500000000000000000, 0.2604166666666666852, 0.2708333333333333148, 0.2812500000000000000, 0.2916666666666666852, 0.3020833333333333148, 0.3125000000000000000, 0.3229166666666666297, 0.3333333333333333148, 0.3437500000000000000, 0.3541666666666666852, 0.3645833333333333148, 0.3750000000000000555, 0.3854166666666666852, 0.3958333333333333148, 0.4062500000000000000, 0.4166666666666666852, 0.4270833333333333148, 0.4375000000000000000, 0.4479166666666666297, 0.4583333333333333148, 0.4687500000000000000, 0.4791666666666666852, 0.4895833333333333148, 0.5000000000000000000, 0.5104166666666666297, 0.5208333333333333703, 0.5312500000000000000, 0.5416666666666666297, 0.5520833333333333703, 0.5625000000000000000, 0.5729166666666666297, 0.5833333333333333703, 0.5937500000000000000, 0.6041666666666666297, 0.6145833333333333703, 0.6250000000000000000, 0.6354166666666666297, 0.6458333333333333703, 0.6562500000000000000, 0.6666666666666666297, 0.6770833333333333703, 0.6875000000000000000, 0.6979166666666667407, 0.7083333333333333703, 0.7187500000000000000, 0.7291666666666666297, 0.7395833333333333703, 0.7500000000000000000, 0.7604166666666666297, 0.7708333333333332593, 0.7812500000000000000, 0.7916666666666666297, 0.8020833333333333703, 0.8125000000000000000, 0.8229166666666666297, 0.8333333333333333703, 0.8437499999999998890, 0.8541666666666666297, 0.8645833333333333703, 0.8750000000000000000, 0.8854166666666666297, 0.8958333333333333703, 0.9062500000000000000, 0.9166666666666667407, 0.9270833333333333703, 0.9375000000000000000 ),
 .UNSPECIFIED. ) 
 CURVE ( )  GEOMETRIC_REPRESENTATION_ITEM ( )  RATIONAL_B_SPLINE_CURVE ( ( 0.9626285260900118157, 0.9670597623776912011, 1.000000000000000000, 0.9238795325112867385, 1.000000000000000000, 0.9238795325112867385, 1.000000000000000000, 0.9238795325112867385, 1.000000000000000000, 0.9238795325112867385, 1.000000000000000000, 0.9238795325112867385, 1.000000000000000000, 0.9238795325112867385, 1.000000000000000000, 0.9238795325112867385, 1.000000000000000000, 0.9238795325112867385, 1.000000000000000000, 0.9238795325112867385, 1.000000000000000000, 0.9238795325112867385, 1.000000000000000000, 0.9238795325112867385, 1.000000000000000000, 0.9238795325112867385, 1.000000000000000000, 0.9238795325112867385, 1.000000000000000000, 0.9238795325112867385, 1.000000000000000000, 0.9238795325112867385, 1.000000000000000000, 0.9238795325112867385, 1.000000000000000000, 0.9238795325112867385, 1.000000000000000000, 0.9238795325112867385, 1.000000000000000000, 0.9238795325112867385, 1.000000000000000000, 0.9238795325112867385, 1.000000000000000000, 0.9238795325112867385, 1.000000000000000000, 0.9238795325112867385, 1.000000000000000000, 0.9238795325112867385, 1.000000000000000000, 0.9238795325112867385, 1.000000000000000000, 0.9238795325112867385, 1.000000000000000000, 0.9238795325112867385, 1.000000000000000000, 0.9238795325112867385, 1.000000000000000000, 0.9238795325112867385, 1.000000000000000000, 0.9238795325112867385, 1.000000000000000000, 0.9238795325112867385, 1.000000000000000000, 0.9238795325112867385, 1.000000000000000000, 0.9238795325112867385, 1.000000000000000000, 0.9238795325112867385, 1.000000000000000000, 0.9238795325112867385, 1.000000000000000000, 0.9238795325112867385, 1.000000000000000000, 0.9238795325112867385, 1.000000000000000000, 0.9238795325112867385, 1.000000000000000000, 0.9238795325112867385, 1.000000000000000000, 0.9238795325112867385, 1.000000000000000000, 0.9238795325112867385, 1.000000000000000000, 0.9238795325112867385, 1.000000000000000000, 0.9238795325112867385, 1.000000000000000000, 0.9238795325112867385, 1.000000000000000000, 0.9238795325112867385, 1.000000000000000000, 0.9238795325112867385, 1.000000000000000000, 0.9238795325112867385, 1.000000000000000000, 0.9238795325112867385, 1.000000000000000000, 0.9238795325112867385, 1.000000000000000000, 0.9238795325112867385, 1.000000000000000000, 0.9238795325112867385, 1.000000000000000000, 0.9238795325112867385, 1.000000000000000000, 0.9238795325112867385, 1.000000000000000000, 0.9238795325112867385, 1.000000000000000000, 0.9238795325112867385, 1.000000000000000000, 0.9238795325112867385, 1.000000000000000000, 0.9238795325112867385, 1.000000000000000000, 0.9238795325112867385, 1.000000000000000000, 0.9238795325112867385, 1.000000000000000000, 0.9238795325112867385, 1.000000000000000000, 0.9238795325112867385, 1.000000000000000000, 0.9238795325112867385, 1.000000000000000000, 0.9238795325112867385, 1.000000000000000000, 0.9238795325112867385, 1.000000000000000000, 0.9238795325112867385, 1.000000000000000000, 0.9238795325112867385, 1.000000000000000000, 0.9238795325112867385, 1.000000000000000000, 0.9238795325112867385, 1.000000000000000000, 0.9238795325112867385, 1.000000000000000000, 0.9238795325112867385, 1.000000000000000000, 0.9238795325112867385, 1.000000000000000000, 0.9238795325112867385, 1.000000000000000000, 0.9238795325112867385, 1.000000000000000000, 0.9238795325112867385, 1.000000000000000000, 0.9238795325112867385, 1.000000000000000000, 0.9238795325112867385, 1.000000000000000000, 0.9238795325112867385, 1.000000000000000000, 0.9238795325112867385, 1.000000000000000000, 0.9238795325112867385, 1.000000000000000000, 0.9238795325112867385, 1.000000000000000000, 0.9238795325112867385, 1.000000000000000000, 0.9238795325112867385, 1.000000000000000000, 0.9238795325112867385, 1.000000000000000000 ) ) 
 REPRESENTATION_ITEM ( '' )  );
#17255 =( BOUNDED_CURVE ( )  B_SPLINE_CURVE ( 2, ( #17675, #17794, #3153, #10247, #12208, #12324, #17555, #21334, #6572 ),
 .UNSPECIFIED., .F., .F. ) 
 B_SPLINE_CURVE_WITH_KNOTS ( ( 3, 2, 2, 2, 3 ),
 ( 0.6979166666666667407, 0.7083333333333333703, 0.7187500000000000000, 0.7291666666666667407, 0.7395833333333333703 ),
 .UNSPECIFIED. ) 
 CURVE ( )  GEOMETRIC_REPRESENTATION_ITEM ( )  RATIONAL_B_SPLINE_CURVE ( ( 1.000000000000000000, 0.9238795325112867385, 1.000000000000000000, 0.9238795325112867385, 1.000000000000000000, 0.9238795325112867385, 1.000000000000000000, 0.9238795325112867385, 1.000000000000000000 ) ) 
 REPRESENTATION_ITEM ( '' )  );
#17256 = DIRECTION ( 'NONE',  ( -0.000000000000000000, -1.000000000000000000, -0.000000000000000000 ) ) ;
#17257 = CARTESIAN_POINT ( 'NONE',  ( -0.07569519822120913954, 5.165236573017851995, -0.2884437376132976683 ) ) ;
#17258 = CARTESIAN_POINT ( 'NONE',  ( 0.1292346314604058410, 4.741750000151731648, 0.3119999999999998885 ) ) ;
#17259 = VECTOR ( 'NONE', #20638, 39.37007874015748854 ) ;
#17260 = CARTESIAN_POINT ( 'NONE',  ( -0.2819296736111110979, 4.922305555631420582, 0.000000000000000000 ) ) ;
#17261 = ORIENTED_EDGE ( 'NONE', *, *, #18463, .F. ) ;
#17262 = CARTESIAN_POINT ( 'NONE',  ( -0.2819296736111110424, 4.182722222298087544, -0.1167790944451423119 ) ) ;
#17263 = ORIENTED_EDGE ( 'NONE', *, *, #4056, .T. ) ;
#17264 = CARTESIAN_POINT ( 'NONE',  ( 0.1116596296178199860, 0.07946428561674331870, -0.3436530038418508792 ) ) ;
#17265 = ORIENTED_EDGE ( 'NONE', *, *, #12577, .F. ) ;
#17266 = VERTEX_POINT ( 'NONE', #274 ) ;
#17267 = PERSON_AND_ORGANIZATION ( #15518, #2538 ) ;
#17268 = CARTESIAN_POINT ( 'NONE',  ( 0.000000000000000000, 0.01999999999999951469, 0.000000000000000000 ) ) ;
#17269 = CARTESIAN_POINT ( 'NONE',  ( 1.617249732617304092, 2.740000000000000213, -2.801158705420349726 ) ) ;
#17270 = CARTESIAN_POINT ( 'NONE',  ( 0.2819296736111111534, 3.835500000075866112, 0.1167790944451422563 ) ) ;
#17271 = CARTESIAN_POINT ( 'NONE',  ( 0.3141711261733516891, 4.418235456225991342, 0.02406080032727062751 ) ) ;
#17272 = CARTESIAN_POINT ( 'NONE',  ( 0.000000000000000000, 3.700000000000000622, 0.000000000000000000 ) ) ;
#17273 = CARTESIAN_POINT ( 'NONE',  ( 0.01848103877824610469, -0.5441716683897390716, 0.04413116910601656145 ) ) ;
#17274 = CARTESIAN_POINT ( 'NONE',  ( -0.1144950937579609779, 0.2764156081756484196, 0.3001388888888924522 ) ) ;
#17275 = CARTESIAN_POINT ( 'NONE',  ( -0.2819296736111111534, 0.4138888888130222155, 0.1167790944451422563 ) ) ;
#17276 = CARTESIAN_POINT ( 'NONE',  ( -0.1954553509668046640, 0.1954553509668046918, -0.1408333333333332826 ) ) ;
#17277 = ORIENTED_EDGE ( 'NONE', *, *, #3221, .T. ) ;
#17278 = CARTESIAN_POINT ( 'NONE',  ( 0.2819296736111110979, 4.838972222298088433, -3.452642723725051716E-17 ) ) ;
#17279 = CARTESIAN_POINT ( 'NONE',  ( 0.1993543840281266633, 4.665361111186976828, -0.1993543840281266910 ) ) ;
#17280 = CARTESIAN_POINT ( 'NONE',  ( 0.4593750000000002554, -1.978974282089605735E-13, 0.4343810118395207698 ) ) ;
#17281 = CARTESIAN_POINT ( 'NONE',  ( 0.2683590975675059220, 4.868055150729749592, -0.1597197667041882485 ) ) ;
#17282 = CARTESIAN_POINT ( 'NONE',  ( -0.3716965727725675683, -7.597319298711556630E-17, 0.1377364605766528416 ) ) ;
#17283 = CARTESIAN_POINT ( 'NONE',  ( 0.2533266501255685976, -0.1176800686430039961, 0.3893196305818418801 ) ) ;
#17284 = CARTESIAN_POINT ( 'NONE',  ( 0.2206173157302027954, 4.363277777777777366, -0.2206173157302028232 ) ) ;
#17285 = CARTESIAN_POINT ( 'NONE',  ( 0.1993543840281267465, 3.762583333409198705, 0.1993543840281266633 ) ) ;
#17286 = EDGE_CURVE ( 'NONE', #9562, #18946, #23717, .T. ) ;
#17287 = PLANE ( 'NONE',  #14735 ) ;
#17288 = ORIENTED_EDGE ( 'NONE', *, *, #20468, .T. ) ;
#17289 = CARTESIAN_POINT ( 'NONE',  ( 0.3107418810063447556, 4.584733417854850224, 0.02800694585020104335 ) ) ;
#17290 = ORIENTED_EDGE ( 'NONE', *, *, #20167, .T. ) ;
#17291 = CARTESIAN_POINT ( 'NONE',  ( 0.04619135323477931848, 4.683997901097691319, 0.3085712561171880530 ) ) ;
#17292 = CARTESIAN_POINT ( 'NONE',  ( 0.4723836327791856582, -0.2801952116499829559, 0.04193567535760548554 ) ) ;
#17293 = CARTESIAN_POINT ( 'NONE',  ( -0.1144950937579609779, 0.2764156081756484196, 0.4112500000000044453 ) ) ;
#17294 = CARTESIAN_POINT ( 'NONE',  ( -0.0005581460392713915100, 3.932738050107600802, -0.3119995721350460882 ) ) ;
#17295 = ORIENTED_EDGE ( 'NONE', *, *, #11414, .F. ) ;
#17296 = CARTESIAN_POINT ( 'NONE',  ( -6.979263641208234666E-17, 0.4223214284738860402, 0.3799334167787516425 ) ) ;
#17297 = CARTESIAN_POINT ( 'NONE',  ( 0.1993543840281266910, 0.4312499999241333759, -0.1993543840281266910 ) ) ;
#17298 = DIRECTION ( 'NONE',  ( 0.000000000000000000, -0.000000000000000000, 1.000000000000000000 ) ) ;
#17299 = CARTESIAN_POINT ( 'NONE',  ( 0.2870356121319265763, 0.3498146942408093540, -1.162598210319561343 ) ) ;
#17300 = CARTESIAN_POINT ( 'NONE',  ( -0.2744310710835944356, -0.1177455570399758150, -0.08727062790145140303 ) ) ;
#17301 = CARTESIAN_POINT ( 'NONE',  ( 0.000000000000000000, 0.2764156081756484196, 0.2480555555555586933 ) ) ;
#17302 = CIRCLE ( 'NONE', #14580, 0.01875000000000003747 ) ;
#17303 = ORIENTED_EDGE ( 'NONE', *, *, #23714, .F. ) ;
#17304 = CARTESIAN_POINT ( 'NONE',  ( -0.1511513228892870098, 4.622670932816259182, 0.2729428619954094581 ) ) ;
#17305 = DIRECTION ( 'NONE',  ( 0.000000000000000000, 0.000000000000000000, 1.000000000000000000 ) ) ;
#17306 = CARTESIAN_POINT ( 'NONE',  ( -0.1174872052320808657, -2.846948999568485577E-18, -0.3695961464677890995 ) ) ;
#17307 = CARTESIAN_POINT ( 'NONE',  ( 0.1292346314604057023, 0.2854166666666662633, 0.3119999999999998885 ) ) ;
#17308 = CARTESIAN_POINT ( 'NONE',  ( 0.2206173157302027954, 4.863277777777777366, -0.2206173157302028232 ) ) ;
#17309 = CARTESIAN_POINT ( 'NONE',  ( -0.1167790944451423535, 4.099388888964754507, 0.2819296736111110424 ) ) ;
#17310 = DIRECTION ( 'NONE',  ( -0.8651979924482607887, 0.04370253788966922681, 0.4995222938423281578 ) ) ;
#17311 = DIRECTION ( 'NONE',  ( 0.000000000000000000, 1.000000000000000000, 0.000000000000000000 ) ) ;
#17312 = LINE ( 'NONE', #19380, #7147 ) ;
#17313 = ORIENTED_EDGE ( 'NONE', *, *, #906, .F. ) ;
#17314 = ORIENTED_EDGE ( 'NONE', *, *, #15741, .T. ) ;
#17315 = CARTESIAN_POINT ( 'NONE',  ( 0.000000000000000000, 5.384999999999999787, 0.000000000000000000 ) ) ;
#17316 = CARTESIAN_POINT ( 'NONE',  ( -1.726321361862525858E-17, 4.838972222298088433, -0.2819296736111110979 ) ) ;
#17317 = CARTESIAN_POINT ( 'NONE',  ( -0.3613381517857143232, 0.3866071427596004528, -4.425116109941954795E-17 ) ) ;
#17318 = CARTESIAN_POINT ( 'NONE',  ( -0.1089525909866506520, 4.512992428746574802, 0.2955693577741866918 ) ) ;
#17319 = CIRCLE ( 'NONE', #18886, 0.01874999999999996461 ) ;
#17320 = PERSON_AND_ORGANIZATION ( #15518, #2538 ) ;
#17321 = CARTESIAN_POINT ( 'NONE',  ( -0.3066867353193435397, 0.9548081934128058723, 2.155722135785137716 ) ) ;
#17322 = PLANE ( 'NONE',  #1742 ) ;
#17323 = CARTESIAN_POINT ( 'NONE',  ( -0.1993543840281266910, 4.415361111186976828, -0.1993543840281266910 ) ) ;
#17324 = EDGE_CURVE ( 'NONE', #16523, #1066, #2946, .T. ) ;
#17325 = B_SPLINE_CURVE_WITH_KNOTS ( 'NONE', 3,
 ( #12246, #8679, #4664, #1132, #17595, #19660, #8317, #23543, #17839, #16128, #5138, #8565, #4904, #14300, #19540, #23302, #21734, #5019, #2719, #15769, #12484, #3193, #23187, #2832, #8800, #16251, #23661, #6980, #15884 ),
 .UNSPECIFIED., .F., .F.,
 ( 4, 2, 1, 1, 1, 2, 2, 2, 2, 2, 2, 2, 2, 2, 2, 4 ),
 ( 0.4299228192795082060, 0.4302011865891702813, 0.4303403702440012912, 0.4304099620714167962, 0.4304447579851246042, 0.4304621559419784527, 0.4304795538988323567, 0.4310362885181565074, 0.4321497577568047532, 0.4343766962341013560, 0.4366036347113979588, 0.4388305731886945615, 0.4410575116659911643, 0.4432844501432877116, 0.4455113886205843143, 0.4477383270978809171 ),
 .UNSPECIFIED. ) ;
#17326 = CARTESIAN_POINT ( 'NONE',  ( 0.3120000000000000551, 4.297305555555554157, 0.1292346314604056190 ) ) ;
#17327 = CARTESIAN_POINT ( 'NONE',  ( 0.1954553509668046640, -0.1954553509668047195, -0.05055555555555479863 ) ) ;
#17328 = APPROVAL_PERSON_ORGANIZATION ( #676, #5204, #19089 ) ;
#17329 = CARTESIAN_POINT ( 'NONE',  ( 0.3394572874457115752, 3.700000000000000622, 0.09499999999999993172 ) ) ;
#17330 = CARTESIAN_POINT ( 'NONE',  ( -0.2819296736111110424, 0.4069444443685779067, -0.1167790944451423396 ) ) ;
#17331 = CARTESIAN_POINT ( 'NONE',  ( -0.4749999999999999778, 3.575000000000000622, 0.09499999999999995948 ) ) ;
#17332 = CARTESIAN_POINT ( 'NONE',  ( -0.2472135954999579444, 0.1392857142857142350, -0.3402603233408160732 ) ) ;
#17333 = LINE ( 'NONE', #627, #2565 ) ;
#17334 = CARTESIAN_POINT ( 'NONE',  ( 0.1306872919485614071, -0.3155070326520293955, 0.1352083333333353732 ) ) ;
#17335 = EDGE_CURVE ( 'NONE', #23444, #18530, #10429, .T. ) ;
#17336 = CARTESIAN_POINT ( 'NONE',  ( 0.1292346314604007063, 3.977861111111111292, -0.3120000000000049400 ) ) ;
#17337 = CARTESIAN_POINT ( 'NONE',  ( 7.043045608665678148E-17, -0.5196152422706635798, 0.4425000000000000044 ) ) ;
#17338 = CARTESIAN_POINT ( 'NONE',  ( 0.2819296736111110979, 0.4243055554796889006, 0.000000000000000000 ) ) ;
#17339 = CARTESIAN_POINT ( 'NONE',  ( -0.1167790944451422702, 0.2749999999241333204, -0.2819296736111110424 ) ) ;
#17340 = CARTESIAN_POINT ( 'NONE',  ( -0.1167790944451423535, 4.210500000075866112, 0.2819296736111110424 ) ) ;
#17341 = CARTESIAN_POINT ( 'NONE',  ( -0.2472135954999579999, 0.2946428569477723691, 0.3402603233408159622 ) ) ;
#17342 = VECTOR ( 'NONE', #19062, 39.37007874015748143 ) ;
#17343 = CARTESIAN_POINT ( 'NONE',  ( -1.726321361862525858E-17, 4.797305555631421470, -0.2819296736111110979 ) ) ;
#17344 = CARTESIAN_POINT ( 'NONE',  ( -0.3125000000000000000, 1.913510623667739771E-17, 0.2897222222222258226 ) ) ;
#17345 = LINE ( 'NONE', #11506, #1546 ) ;
#17346 = CARTESIAN_POINT ( 'NONE',  ( 0.3119999999999999996, 3.755638889040621375, -0.1292346314604056745 ) ) ;
#17347 = CARTESIAN_POINT ( 'NONE',  ( 0.000000000000000000, 2.740000000000000213, -0.05000000000000028727 ) ) ;
#17348 =( LENGTH_UNIT ( ) NAMED_UNIT ( * ) SI_UNIT ( $, .METRE. ) );
#17349 = ORIENTED_EDGE ( 'NONE', *, *, #5269, .F. ) ;
#17350 = EDGE_CURVE ( 'NONE', #45, #17046, #2708, .T. ) ;
#17351 = EDGE_CURVE ( 'NONE', #11042, #13964, #2154, .T. ) ;
#17352 = B_SPLINE_CURVE_WITH_KNOTS ( 'NONE', 3,
 ( #2975, #11024, #13109, #18088, #22225, #18448, #1509, #12748, #5157, #20164, #5402, #5645, #21866, #18215, #12867, #23923, #21986, #1388, #22343, #10657 ),
 .UNSPECIFIED., .F., .F.,
 ( 4, 2, 2, 2, 2, 2, 2, 2, 2, 4 ),
 ( 0.1918878366009665604, 0.1930301452378265503, 0.1941724538746865680, 0.1964570711484065479, 0.1987416884221265556, 0.2010263056958465633, 0.2033109229695665710, 0.2055955402432865509, 0.2078801575170065585, 0.2101647747907265662 ),
 .UNSPECIFIED. ) ;
#17353 = PERSON_AND_ORGANIZATION_ROLE ( 'design_owner' ) ;
#17354 = VECTOR ( 'NONE', #1042, 39.37007874015748143 ) ;
#17355 = CARTESIAN_POINT ( 'NONE',  ( 0.1236067977499789028, 0.4482142855192008946, 0.3804226065180614791 ) ) ;
#17356 = CARTESIAN_POINT ( 'NONE',  ( -0.2306026292281220802, 5.008719013999844094, 0.2101591525671422378 ) ) ;
#17357 = ORIENTED_EDGE ( 'NONE', *, *, #16892, .T. ) ;
#17358 = CARTESIAN_POINT ( 'NONE',  ( -0.2819296736111110979, 0.08055555547968892838, 0.1167790944451422425 ) ) ;
#17359 = VERTEX_POINT ( 'NONE', #2593 ) ;
#17360 = CARTESIAN_POINT ( 'NONE',  ( -0.4000000000000000222, 0.01071428571428569530, 0.1299678784931624920 ) ) ;
#17361 = LINE ( 'NONE', #16997, #17842 ) ;
#17362 = CARTESIAN_POINT ( 'NONE',  ( 0.01044473586599018768, 4.765759009506619570, -0.3118501016267402060 ) ) ;
#17363 = CARTESIAN_POINT ( 'NONE',  ( 0.2923287055106771337, 0.2866071427596004195, -0.2123892367102620249 ) ) ;
#17364 = CARTESIAN_POINT ( 'NONE',  ( 0.04801364120717823564, 5.189167739831288984, -0.2857187088061001190 ) ) ;
#17365 = EDGE_CURVE ( 'NONE', #11401, #13845, #12587, .T. ) ;
#17366 = ORIENTED_EDGE ( 'NONE', *, *, #16516, .T. ) ;
#17367 = LOCAL_TIME ( 21, 9, 13.00000000000000000, #12130 ) ;
#17368 = CARTESIAN_POINT ( 'NONE',  ( 0.7108475124358174524, 0.9548081934128058723, 2.743195807636230388 ) ) ;
#17369 = CARTESIAN_POINT ( 'NONE',  ( -0.2338143246629017236, 4.675255141077020227, 0.2066237434125970107 ) ) ;
#17370 = CARTESIAN_POINT ( 'NONE',  ( 0.1993543840281266633, 4.109805555631420582, -0.1993543840281266910 ) ) ;
#17371 = CARTESIAN_POINT ( 'NONE',  ( -5.308788303787306404E-17, 0.03949697488198145034, 0.2889969748819818385 ) ) ;
#17372 = CARTESIAN_POINT ( 'NONE',  ( -0.1166234456863257940, 4.111524471938507119, -2.802594437230254254 ) ) ;
#17373 = AXIS2_PLACEMENT_3D ( 'NONE', #6217, #21570, #12329 ) ;
#17374 = CARTESIAN_POINT ( 'NONE',  ( -0.3119999999999999996, 4.446611111262843252, 0.000000000000000000 ) ) ;
#17375 = CARTESIAN_POINT ( 'NONE',  ( 0.2819296736111110979, 4.894527777853643791, -3.452642723725051716E-17 ) ) ;
#17376 = ORIENTED_EDGE ( 'NONE', *, *, #23780, .T. ) ;
#17377 = CARTESIAN_POINT ( 'NONE',  ( -1.726321361862525858E-17, 4.005638888964754507, -0.2819296736111110979 ) ) ;
#17378 = ORIENTED_EDGE ( 'NONE', *, *, #22827, .F. ) ;
#17379 = EDGE_CURVE ( 'NONE', #14283, #5468, #4771, .T. ) ;
#17380 = EDGE_CURVE ( 'NONE', #4599, #16588, #21308, .T. ) ;
#17381 = VERTEX_POINT ( 'NONE', #5007 ) ;
#17382 = CALENDAR_DATE ( 2026, 7, 10 ) ;
#17383 = ORIENTED_EDGE ( 'NONE', *, *, #16842, .T. ) ;
#17384 = DIRECTION ( 'NONE',  ( -1.000000000000000000, 0.000000000000000000, 0.000000000000000000 ) ) ;
#17385 = CARTESIAN_POINT ( 'NONE',  ( 0.08808798601665612793, 3.066692553488282957, 3.256612888476066558 ) ) ;
#17386 = CARTESIAN_POINT ( 'NONE',  ( -0.1292346314604056190, 0.08402777762604483891, -0.3119999999999999996 ) ) ;
#17387 = AXIS2_PLACEMENT_3D ( 'NONE', #15846, #1779, #17796 ) ;
#17388 = CARTESIAN_POINT ( 'NONE',  ( 0.08315995787118272975, 4.407302845992192353, 0.3007856028562817530 ) ) ;
#17389 = EDGE_CURVE ( 'NONE', #2851, #5871, #20750, .T. ) ;
#17390 =( BOUNDED_CURVE ( )  B_SPLINE_CURVE ( 2, ( #17211, #2458, #7818, #20979, #11730, #8051, #17327, #22573, #18920, #17088, #21104, #15501, #495, #739, #5861, #15622, #4393, #22927, #20862, #3920, #2574, #11486, #11365, #377, #2220, #5980, #15260, #13443, #257, #10024, #7697, #11855, #13320, #20742, #19269, #5749, #7928, #13208, #22810, #2341, #17446, #9777, #18792, #4156, #22690, #6101, #2087, #15382, #15143, #6464, #8530, #23395, #12452, #18043, #21463, #2691, #21225, #10144, #14033, #23511, #17926, #3049, #19511, #21576, #8405, #4514, #6584, #2925, #6702, #12337, #19871, #3163, #21346, #2804, #19754, #10259, #4634, #10613, #4747, #4870, #17568, #12218, #10496, #15743, #19628, #1339, #4988, #10385, #17685, #12101, #17807, #977, #11980, #6345, #15855, #23272, #1098, #15974, #14147, #1222, #8648, #16097, #6826, #14267, #21704, #8768, #23040, #13797, #19393, #858, #8289, #23153, #13918, #13383, #6951, #5353, #15203, #22639, #320, #11552, #16459, #10734, #3406, #4094, #18522, #19993, #10978, #24000, #7074, #7191, #3527, #12943, #20237, #20355, #18404 ),
 .UNSPECIFIED., .F., .F. ) 
 B_SPLINE_CURVE_WITH_KNOTS ( ( 3, 2, 2, 2, 2, 2, 2, 2, 2, 2, 2, 2, 2, 2, 2, 2, 2, 2, 2, 2, 2, 2, 2, 2, 2, 2, 2, 2, 2, 2, 2, 2, 2, 2, 2, 2, 2, 2, 2, 2, 2, 2, 2, 2, 2, 2, 2, 2, 2, 2, 2, 2, 2, 2, 2, 2, 2, 2, 2, 2, 2, 2, 2, 2, 2, 2, 2, 3 ),
 ( 0.1128009810283470138, 0.1145833333333333287, 0.1250000000000000000, 0.1354166666666666574, 0.1458333333333333426, 0.1562500000000000000, 0.1666666666666666574, 0.1770833333333333426, 0.1875000000000000000, 0.1979166666666666574, 0.2083333333333333703, 0.2187500000000000000, 0.2291666666666666574, 0.2395833333333333426, 0.2500000000000000000, 0.2604166666666666852, 0.2708333333333333148, 0.2812500000000000000, 0.2916666666666666852, 0.3020833333333333703, 0.3125000000000000000, 0.3229166666666666297, 0.3333333333333333703, 0.3437500000000000000, 0.3541666666666667407, 0.3645833333333333148, 0.3750000000000000000, 0.3854166666666666852, 0.3958333333333333148, 0.4062500000000000000, 0.4166666666666666852, 0.4270833333333333148, 0.4375000000000000000, 0.4479166666666666852, 0.4583333333333333148, 0.4687500000000000000, 0.4791666666666666852, 0.4895833333333333703, 0.4999999999999999445, 0.5104166666666665186, 0.5208333333333333703, 0.5312500000000000000, 0.5416666666666666297, 0.5520833333333332593, 0.5625000000000000000, 0.5729166666666667407, 0.5833333333333333703, 0.5937500000000000000, 0.6041666666666666297, 0.6145833333333333703, 0.6250000000000000000, 0.6354166666666666297, 0.6458333333333333703, 0.6562500000000000000, 0.6666666666666666297, 0.6770833333333333703, 0.6875000000000000000, 0.6979166666666666297, 0.7083333333333333703, 0.7187500000000000000, 0.7291666666666666297, 0.7395833333333333703, 0.7500000000000000000, 0.7604166666666666297, 0.7708333333333333703, 0.7812500000000000000, 0.7916666666666666297, 0.7934490189716459918 ),
 .UNSPECIFIED. ) 
 CURVE ( )  GEOMETRIC_REPRESENTATION_ITEM ( )  RATIONAL_B_SPLINE_CURVE ( ( 0.9784078784059424549, 0.9869753448942262253, 1.000000000000000000, 0.9238795325112867385, 1.000000000000000000, 0.9238795325112867385, 1.000000000000000000, 0.9238795325112867385, 1.000000000000000000, 0.9238795325112867385, 1.000000000000000000, 0.9238795325112867385, 1.000000000000000000, 0.9238795325112867385, 1.000000000000000000, 0.9238795325112867385, 1.000000000000000000, 0.9238795325112867385, 1.000000000000000000, 0.9238795325112867385, 1.000000000000000000, 0.9238795325112867385, 1.000000000000000000, 0.9238795325112867385, 1.000000000000000000, 0.9238795325112867385, 1.000000000000000000, 0.9238795325112867385, 1.000000000000000000, 0.9238795325112867385, 1.000000000000000000, 0.9238795325112867385, 1.000000000000000000, 0.9238795325112867385, 1.000000000000000000, 0.9238795325112867385, 1.000000000000000000, 0.9238795325112867385, 1.000000000000000000, 0.9238795325112867385, 1.000000000000000000, 0.9238795325112867385, 1.000000000000000000, 0.9238795325112867385, 1.000000000000000000, 0.9238795325112867385, 1.000000000000000000, 0.9238795325112867385, 1.000000000000000000, 0.9238795325112867385, 1.000000000000000000, 0.9238795325112867385, 1.000000000000000000, 0.9238795325112867385, 1.000000000000000000, 0.9238795325112867385, 1.000000000000000000, 0.9238795325112867385, 1.000000000000000000, 0.9238795325112867385, 1.000000000000000000, 0.9238795325112867385, 1.000000000000000000, 0.9238795325112867385, 1.000000000000000000, 0.9238795325112867385, 1.000000000000000000, 0.9238795325112867385, 1.000000000000000000, 0.9238795325112867385, 1.000000000000000000, 0.9238795325112867385, 1.000000000000000000, 0.9238795325112867385, 1.000000000000000000, 0.9238795325112867385, 1.000000000000000000, 0.9238795325112867385, 1.000000000000000000, 0.9238795325112867385, 1.000000000000000000, 0.9238795325112867385, 1.000000000000000000, 0.9238795325112867385, 1.000000000000000000, 0.9238795325112867385, 1.000000000000000000, 0.9238795325112867385, 1.000000000000000000, 0.9238795325112867385, 1.000000000000000000, 0.9238795325112867385, 1.000000000000000000, 0.9238795325112867385, 1.000000000000000000, 0.9238795325112867385, 1.000000000000000000, 0.9238795325112867385, 1.000000000000000000, 0.9238795325112867385, 1.000000000000000000, 0.9238795325112867385, 1.000000000000000000, 0.9238795325112867385, 1.000000000000000000, 0.9238795325112867385, 1.000000000000000000, 0.9238795325112867385, 1.000000000000000000, 0.9238795325112867385, 1.000000000000000000, 0.9238795325112867385, 1.000000000000000000, 0.9238795325112867385, 1.000000000000000000, 0.9238795325112867385, 1.000000000000000000, 0.9238795325112867385, 1.000000000000000000, 0.9238795325112867385, 1.000000000000000000, 0.9238795325112867385, 1.000000000000000000, 0.9238795325112867385, 1.000000000000000000, 0.9238795325112867385, 1.000000000000000000, 0.9238795325112867385, 1.000000000000000000, 0.9238795325112867385, 1.000000000000000000, 0.9238795325112867385, 1.000000000000000000, 0.9869753448942770735, 0.9784078784060095124 ) ) 
 REPRESENTATION_ITEM ( '' )  );
#17391 = CARTESIAN_POINT ( 'NONE',  ( 0.2725578398252748724, -0.3839045351724091337, 0.09139393128962809698 ) ) ;
#17392 = CARTESIAN_POINT ( 'NONE',  ( -0.1954553509668046918, -0.1954553509668046640, 0.3175000000000037237 ) ) ;
#17393 = CARTESIAN_POINT ( 'NONE',  ( 0.1993543840281266910, 0.3895833332574667462, -0.1993543840281266910 ) ) ;
#17394 = CARTESIAN_POINT ( 'NONE',  ( 0.2764156081756483641, -0.1144950937579611167, 0.3973611111111153837 ) ) ;
#17395 = ORIENTED_EDGE ( 'NONE', *, *, #21395, .F. ) ;
#17396 = CARTESIAN_POINT ( 'NONE',  ( -0.1993543840281266355, 4.818138888964754507, 0.1993543840281267465 ) ) ;
#17397 = CARTESIAN_POINT ( 'NONE',  ( 0.3999999999999999667, -0.03392857162365620766, -0.1299678784931625475 ) ) ;
#17398 = CARTESIAN_POINT ( 'NONE',  ( 0.1167790944451424368, 4.592444444520309865, 0.2819296736111110424 ) ) ;
#17399 = LINE ( 'NONE', #4589, #5618 ) ;
#17400 = CARTESIAN_POINT ( 'NONE',  ( 0.1294417382415921358, -0.3125000000000002220, 0.3556944444444482545 ) ) ;
#17401 = CARTESIAN_POINT ( 'NONE',  ( -0.3508668692247319254, -2.437189573335655702E-18, 0.1793730417398099186 ) ) ;
#17402 = CARTESIAN_POINT ( 'NONE',  ( -0.4593750000000004219, 0.2760455974562897596, 0.06112444011295372487 ) ) ;
#17403 = CARTESIAN_POINT ( 'NONE',  ( -0.3119999999999999996, 4.328555555555554157, 0.000000000000000000 ) ) ;
#17404 = B_SPLINE_CURVE_WITH_KNOTS ( 'NONE', 3,
 ( #10561, #12399, #22001, #15910, #14332, #23816, #14578, #8961, #10919, #1285, #18109, #6765, #23332, #19816, #14211, #16161, #21644, #23577, #19691, #5301, #12275, #5051, #3349, #12520, #10803, #6892, #6644, #17993, #1041, #3113, #21882, #21765, #16408, #19939, #23456, #3227, #16042, #2995, #18231, #8834, #8470, #10445, #1406, #16282, #7017 ),
 .UNSPECIFIED., .F., .F.,
 ( 4, 2, 2, 2, 2, 2, 2, 2, 2, 1, 1, 2, 2, 2, 2, 2, 2, 2, 2, 1, 1, 1, 1, 1, 2, 4 ),
 ( 0.5391066853785936308, 0.5413919047289608155, 0.5436771240793280002, 0.5448197337545115371, 0.5459623434296951849, 0.5482475627800622586, 0.5505327821304294433, 0.5516753918056130912, 0.5522466966432048041, 0.5525323490620007716, 0.5526037621666997079, 0.5526394687190492316, 0.5526751752713986443, 0.5528180014807966280, 0.5539606111559801649, 0.5551032208311637017, 0.5562458305063472386, 0.5568171353439390625, 0.5571027877627349190, 0.5572456139721327917, 0.5573170270768318391, 0.5573527336291812517, 0.5573705869053560136, 0.5573795135434433945, 0.5573839768624870850, 0.5573884401815307754 ),
 .UNSPECIFIED. ) ;
#17405 = CARTESIAN_POINT ( 'NONE',  ( -0.1292346314604056745, 5.158416666818399499, -0.3119999999999999996 ) ) ;
#17406 = CARTESIAN_POINT ( 'NONE',  ( -0.3119999999999999996, 3.995222222222221120, 0.000000000000000000 ) ) ;
#17407 = ORIENTED_EDGE ( 'NONE', *, *, #11843, .T. ) ;
#17408 = AXIS2_PLACEMENT_3D ( 'NONE', #16966, #19155, #5865 ) ;
#17409 = DIRECTION ( 'NONE',  ( 0.000000000000000000, 0.000000000000000000, 1.000000000000000000 ) ) ;
#17410 = ORIENTED_EDGE ( 'NONE', *, *, #21645, .T. ) ;
#17411 = DIRECTION ( 'NONE',  ( 0.000000000000000000, 0.2773500981126144627, 0.9607689228305228424 ) ) ;
#17412 = CARTESIAN_POINT ( 'NONE',  ( 0.05857570580426915696, 4.128840535618094165, 0.3073945904191558998 ) ) ;
#17413 = CARTESIAN_POINT ( 'NONE',  ( 0.000000000000000000, 0.2764156081756484196, 0.4633333333333382043 ) ) ;
#17414 = EDGE_CURVE ( 'NONE', #21824, #2780, #3542, .T. ) ;
#17415 = CARTESIAN_POINT ( 'NONE',  ( -0.2494959594970509731, 3.940827237094480573, -0.1917387026992011523 ) ) ;
#17416 = CARTESIAN_POINT ( 'NONE',  ( 0.1116596296178199027, 0.05089285704531473081, 0.3436530038418508792 ) ) ;
#17417 = AXIS2_PLACEMENT_3D ( 'NONE', #1195, #6800, #10230 ) ;
#17418 = CARTESIAN_POINT ( 'NONE',  ( -0.2819296736111110979, 0.3965277777019111660, -3.452642723725051716E-17 ) ) ;
#17419 = CARTESIAN_POINT ( 'NONE',  ( 0.000000000000000000, 5.384999999999999787, 0.000000000000000000 ) ) ;
#17420 = DIRECTION ( 'NONE',  ( 0.08715574274765830465, -0.9961946980917454342, -3.870492493070289564E-17 ) ) ;
#17421 = CARTESIAN_POINT ( 'NONE',  ( -0.2659300498200202756, -0.1330428112939968099, -0.08601205871610874409 ) ) ;
#17422 = CARTESIAN_POINT ( 'NONE',  ( 0.1954553509668047195, 0.1954553509668046085, 0.1855555555555581937 ) ) ;
#17423 = ORIENTED_EDGE ( 'NONE', *, *, #22272, .F. ) ;
#17424 = CARTESIAN_POINT ( 'NONE',  ( -0.08034884895360394630, 5.116190661212350221, 0.2985391448300075967 ) ) ;
#17425 = LINE ( 'NONE', #8267, #17535 ) ;
#17426 = DIRECTION ( 'NONE',  ( 1.224646799147353207E-16, 0.000000000000000000, -1.000000000000000000 ) ) ;
#17427 = CARTESIAN_POINT ( 'NONE',  ( -0.3119999999999999996, 0.3270833333333330040, 0.1292346314604056190 ) ) ;
#17428 = CARTESIAN_POINT ( 'NONE',  ( -0.1292346314604057023, 4.838972222222222008, 0.3119999999999998885 ) ) ;
#17429 = CARTESIAN_POINT ( 'NONE',  ( -0.1993543840281266910, 3.915361111186976384, -0.1993543840281266910 ) ) ;
#17430 = CARTESIAN_POINT ( 'NONE',  ( -0.08169358551447852834, 4.323948374030631925, -0.3038737831921874410 ) ) ;
#17431 = CARTESIAN_POINT ( 'NONE',  ( -0.07520958173006352110, 0.4863159908245682228, 0.4165421425001717970 ) ) ;
#17432 = CARTESIAN_POINT ( 'NONE',  ( 0.3108775578575657672, 4.806999315166346598, 0.02644136358318530111 ) ) ;
#17433 = ORIENTED_EDGE ( 'NONE', *, *, #16064, .T. ) ;
#17434 = CARTESIAN_POINT ( 'NONE',  ( -0.3120000026603148569, 4.003392929080275664, 0.04084068248537378598 ) ) ;
#17435 = CARTESIAN_POINT ( 'NONE',  ( -0.2819296736111110979, 4.686194444520309865, 0.000000000000000000 ) ) ;
#17436 = CARTESIAN_POINT ( 'NONE',  ( -0.2923287055106771337, 0.3794642856167432798, -0.2123892367102620804 ) ) ;
#17437 = CARTESIAN_POINT ( 'NONE',  ( -0.1292346314604081170, 4.095916666666666650, -0.3119999999999975016 ) ) ;
#17438 = VECTOR ( 'NONE', #15757, 39.37007874015748143 ) ;
#17439 = DIRECTION ( 'NONE',  ( 1.000000000000000000, 0.000000000000000000, 0.000000000000000000 ) ) ;
#17440 = CARTESIAN_POINT ( 'NONE',  ( -0.4687500000000003886, -0.08780557671060627845, 0.08855765995869291363 ) ) ;
#17441 = APPROVAL ( #15672, 'UNSPECIFIED' ) ;
#17442 = CARTESIAN_POINT ( 'NONE',  ( -0.2998642343065030524, 0.08796414601291394075, -0.1016666666666771329 ) ) ;
#17443 = CARTESIAN_POINT ( 'NONE',  ( -0.1993543840281266355, 4.262583333409199149, 0.1993543840281267465 ) ) ;
#17444 = CALENDAR_DATE ( 2026, 7, 10 ) ;
#17445 = CARTESIAN_POINT ( 'NONE',  ( -0.1405978645015776851, 4.047927364732167632, -0.2794846453526392827 ) ) ;
#17446 = CARTESIAN_POINT ( 'NONE',  ( 0.2764156081756484196, -5.077672346800151106E-17, 0.06750000000000168365 ) ) ;
#17447 = CARTESIAN_POINT ( 'NONE',  ( 0.000000000000000000, 3.700000000000000622, -0.7199999999999994182 ) ) ;
#17448 = CARTESIAN_POINT ( 'NONE',  ( 0.1167790944451423257, 0.4486111110352444808, -0.2819296736111110424 ) ) ;
#17449 = LINE ( 'NONE', #743, #21305 ) ;
#17450 = CARTESIAN_POINT ( 'NONE',  ( -0.2472135954999579999, 0.1607142857142856429, 0.3402603233408160732 ) ) ;
#17451 = FACE_OUTER_BOUND ( 'NONE', #16414, .T. ) ;
#17452 = CARTESIAN_POINT ( 'NONE',  ( -0.2230971623002953874, 0.2230971623002954152, 0.1664583333333356230 ) ) ;
#17453 = ORIENTED_EDGE ( 'NONE', *, *, #19594, .F. ) ;
#17454 = DIRECTION ( 'NONE',  ( 0.000000000000000000, 0.000000000000000000, -1.000000000000000000 ) ) ;
#17455 = CARTESIAN_POINT ( 'NONE',  ( 0.000000000000000000, 5.384999999999999787, -0.3119999999999999996 ) ) ;
#17456 = CARTESIAN_POINT ( 'NONE',  ( 0.1167790944451423535, 0.5249999999241333759, 0.2819296736111110979 ) ) ;
#17457 = CARTESIAN_POINT ( 'NONE',  ( -0.1993543840281266633, 0.1673611110352444808, -0.1993543840281266910 ) ) ;
#17458 = CARTESIAN_POINT ( 'NONE',  ( 0.2819296736111110979, 4.172305555631421470, -3.452642723725051716E-17 ) ) ;
#17459 = CARTESIAN_POINT ( 'NONE',  ( 0.2472135954999579166, 0.2374999998049151795, 0.3402603233408160732 ) ) ;
#17460 = CARTESIAN_POINT ( 'NONE',  ( 0.1993543840281267465, 4.554250000075866112, 0.1993543840281266633 ) ) ;
#17461 = EDGE_CURVE ( 'NONE', #5470, #8054, #5125, .T. ) ;
#17462 = ORIENTED_EDGE ( 'NONE', *, *, #4937, .F. ) ;
#17463 = ORIENTED_EDGE ( 'NONE', *, *, #5875, .T. ) ;
#17464 = CARTESIAN_POINT ( 'NONE',  ( -3.827021247335479543E-17, -0.3125000000000000000, 0.2411111111111140515 ) ) ;
#17465 = EDGE_CURVE ( 'NONE', #16467, #14348, #23775, .T. ) ;
#17466 = CARTESIAN_POINT ( 'NONE',  ( -0.2206173157302027676, 3.786888889040620931, 0.2206173157302028787 ) ) ;
#17467 = CARTESIAN_POINT ( 'NONE',  ( -0.04611292249197078419, 0.5146425691514149303, 0.3901966308178845266 ) ) ;
#17468 = CC_DESIGN_PERSON_AND_ORGANIZATION_ASSIGNMENT ( #3222, #1636, ( #17744 ) ) ;
#17469 =( CONVERSION_BASED_UNIT ( 'INCH', #19415 ) LENGTH_UNIT ( ) NAMED_UNIT ( #22851 ) );
#17470 = CARTESIAN_POINT ( 'NONE',  ( 0.2335501899993391861, 0.03242967361111066815, 0.1585748220631333916 ) ) ;
#17471 = AXIS2_PLACEMENT_3D ( 'NONE', #621, #9897, #9529 ) ;
#17472 = DATE_AND_TIME ( #9555, #13110 ) ;
#17473 = CARTESIAN_POINT ( 'NONE',  ( 0.000000000000000000, 6.000000000000000888, 0.000000000000000000 ) ) ;
#17474 = CARTESIAN_POINT ( 'NONE',  ( -0.5116234456863258950, 1.828961980248579033, -2.640781157734872320 ) ) ;
#17475 = EDGE_LOOP ( 'NONE', ( #19959, #23541, #21307, #337 ) ) ;
#17476 = CARTESIAN_POINT ( 'NONE',  ( -0.2819296736111110424, 0.07361111103524449473, -0.1167790944451423396 ) ) ;
#17477 = ORIENTED_EDGE ( 'NONE', *, *, #6913, .T. ) ;
#17478 = CARTESIAN_POINT ( 'NONE',  ( 0.2785718490593341867, 4.256318101036998591, -0.1406648866877419080 ) ) ;
#17479 = CARTESIAN_POINT ( 'NONE',  ( 0.4581189881604794678, 0.2644951211353318010, 0.3941886329748525153 ) ) ;
#17480 = CARTESIAN_POINT ( 'NONE',  ( 0.3019181685026062767, 4.083273234461733736, 0.07867355378959554890 ) ) ;
#17481 = CARTESIAN_POINT ( 'NONE',  ( -0.2923287055106771337, 0.3794642856167432798, -0.2123892367102620804 ) ) ;
#17482 = CARTESIAN_POINT ( 'NONE',  ( 0.2910291928836289399, 5.177951985364569687, 0.04151328995014030854 ) ) ;
#17483 = CARTESIAN_POINT ( 'NONE',  ( -0.2923287055106771337, 0.3973214284738861291, -0.2123892367102620804 ) ) ;
#17484 = CARTESIAN_POINT ( 'NONE',  ( 0.2819296736111110424, 4.050777777853642903, -0.1167790944451423396 ) ) ;
#17485 = DIRECTION ( 'NONE',  ( 0.8660254037844438146, 0.000000000000000000, 0.4999999999999910627 ) ) ;
#17486 = FACE_OUTER_BOUND ( 'NONE', #5361, .T. ) ;
#17487 = AXIS2_PLACEMENT_3D ( 'NONE', #23222, #15568, #10208 ) ;
#17488 = PLANE ( 'NONE',  #2693 ) ;
#17489 = ADVANCED_FACE ( 'NONE', ( #3182 ), #1830, .F. ) ;
#17490 = CARTESIAN_POINT ( 'NONE',  ( 5.731347020009612645E-17, 4.571611111262843252, 0.3119999999999999996 ) ) ;
#17491 = CARTESIAN_POINT ( 'NONE',  ( -0.1167790944451423119, 4.911888888964754507, -0.2819296736111110979 ) ) ;
#17492 = ORIENTED_EDGE ( 'NONE', *, *, #6401, .F. ) ;
#17493 = CARTESIAN_POINT ( 'NONE',  ( -0.1167790944451423257, 3.953555555631421914, -0.2819296736111110424 ) ) ;
#17494 = CARTESIAN_POINT ( 'NONE',  ( -0.2923287055106771337, 0.2508928570453147211, 0.2123892367102619971 ) ) ;
#17495 = ADVANCED_FACE ( 'NONE', ( #21953 ), #1668, .T. ) ;
#17496 = ORIENTED_EDGE ( 'NONE', *, *, #12302, .T. ) ;
#17497 = EDGE_LOOP ( 'NONE', ( #19932, #1991 ) ) ;
#17498 = APPLICATION_PROTOCOL_DEFINITION ( 'international standard', 'config_control_design', 1994, #23822 ) ;
#17499 = ORIENTED_EDGE ( 'NONE', *, *, #6670, .T. ) ;
#17500 = DIRECTION ( 'NONE',  ( -1.000000000000000000, 0.000000000000000000, 0.000000000000000000 ) ) ;
#17501 = CARTESIAN_POINT ( 'NONE',  ( -5.731347020009612645E-17, 0.1638888887371559577, 0.3119999999999999996 ) ) ;
#17502 = VECTOR ( 'NONE', #2182, 39.37007874015748854 ) ;
#17503 = CARTESIAN_POINT ( 'NONE',  ( 0.2283503518066058724, 5.138631362716698625, 0.2031935853610007670 ) ) ;
#17504 = CARTESIAN_POINT ( 'NONE',  ( -1.910449006669871087E-17, 3.759111111111109960, -0.3119999999999999996 ) ) ;
#17505 = CARTESIAN_POINT ( 'NONE',  ( 0.3125000000000000000, -5.740531871003217465E-17, -0.07138888888888809958 ) ) ;
#17506 = PLANE ( 'NONE',  #10267 ) ;
#17507 = CARTESIAN_POINT ( 'NONE',  ( 0.3119999999999998885, 0.2298611109593781954, 0.1292346314604058410 ) ) ;
#17508 = CARTESIAN_POINT ( 'NONE',  ( -0.1167790944451424506, 0.1291666665908000611, 0.2819296736111110424 ) ) ;
#17509 = CARTESIAN_POINT ( 'NONE',  ( 0.2764156081756483641, -0.1144950937579611167, 0.05708333333333497073 ) ) ;
#17510 = ORIENTED_EDGE ( 'NONE', *, *, #17528, .T. ) ;
#17511 = CARTESIAN_POINT ( 'NONE',  ( 0.1167790944451424368, 4.661888888964754507, 0.2819296736111110424 ) ) ;
#17512 = CARTESIAN_POINT ( 'NONE',  ( 1.726321361862525858E-17, 0.6048611110352445364, -0.2819296736111110979 ) ) ;
#17513 = CARTESIAN_POINT ( 'NONE',  ( 0.2819296736111110979, 4.710500000075865223, 0.1167790944451422425 ) ) ;
#17514 = CARTESIAN_POINT ( 'NONE',  ( 0.3119999999999999996, 0.2923611109593781676, -0.1292346314604056468 ) ) ;
#17515 = EDGE_CURVE ( 'NONE', #4879, #2744, #14411, .T. ) ;
#17516 = CARTESIAN_POINT ( 'NONE',  ( -0.08208998203245540526, 0.1891853512034874507, -1.237990233360560355 ) ) ;
#17517 = CARTESIAN_POINT ( 'NONE',  ( -0.3250209672954003093, 7.507838726391275300E-19, 0.2186444650204283358 ) ) ;
#17518 = FACE_OUTER_BOUND ( 'NONE', #20970, .T. ) ;
#17519 = CARTESIAN_POINT ( 'NONE',  ( -0.3119999999999998885, 4.276472222222222008, 0.1292346314604058410 ) ) ;
#17520 = EDGE_CURVE ( 'NONE', #5177, #16467, #20373, .T. ) ;
#17521 = CARTESIAN_POINT ( 'NONE',  ( 0.3119999999999999996, 5.085500000151732536, -3.820898013339742174E-17 ) ) ;
#17522 = CARTESIAN_POINT ( 'NONE',  ( 0.3124206838852614521, 4.975230585218538337, -0.02986472433748768238 ) ) ;
#17523 = CIRCLE ( 'NONE', #5098, 0.2510000000000000009 ) ;
#17524 = AXIS2_PLACEMENT_3D ( 'NONE', #3604, #18484, #1778 ) ;
#17525 = ORIENTED_EDGE ( 'NONE', *, *, #23584, .T. ) ;
#17526 = DIRECTION ( 'NONE',  ( -1.000000000000000000, 0.000000000000000000, 0.000000000000000000 ) ) ;
#17527 = ORIENTED_EDGE ( 'NONE', *, *, #6337, .T. ) ;
#17528 = EDGE_CURVE ( 'NONE', #7579, #21713, #22075, .T. ) ;
#17529 = MANIFOLD_SOLID_BREP ( '1/2-13 Tapped Hole1', #2577 ) ;
#17530 = CARTESIAN_POINT ( 'NONE',  ( 0.1675047463445451801, 4.705591268795053850, -0.2640365305035814458 ) ) ;
#17531 = UNCERTAINTY_MEASURE_WITH_UNIT (LENGTH_MEASURE( 1.000000000000000082E-05 ), #20141, 'distance_accuracy_value', 'NONE');
#17532 = CARTESIAN_POINT ( 'NONE',  ( 0.1823287098769104386, 4.132714727220042406, 0.2533747461830617720 ) ) ;
#17533 = CARTESIAN_POINT ( 'NONE',  ( -0.1306872919485615459, -0.3155070326520293400, 0.1317361111111135519 ) ) ;
#17534 = CARTESIAN_POINT ( 'NONE',  ( -0.2723952011404802698, -0.3839984346608560917, 0.09139143879391148362 ) ) ;
#17535 = VECTOR ( 'NONE', #4017, 39.37007874015748143 ) ;
#17536 = CARTESIAN_POINT ( 'NONE',  ( 0.2923287055106771337, -0.07053571438325667575, -0.2123892367102620249 ) ) ;
#17537 = VECTOR ( 'NONE', #11462, 39.37007874015748854 ) ;
#17538 = CARTESIAN_POINT ( 'NONE',  ( 0.000000000000000000, 3.738758431839877614E-19, -0.1145082521472477743 ) ) ;
#17539 = CARTESIAN_POINT ( 'NONE',  ( 0.3950000000000000178, 2.665000000000000036, -0.2605837454876624437 ) ) ;
#17540 = DIRECTION ( 'NONE',  ( 0.000000000000000000, 0.000000000000000000, 1.000000000000000000 ) ) ;
#17541 = CYLINDRICAL_SURFACE ( 'NONE', #15589, 0.3119999999999999996 ) ;
#17542 = CARTESIAN_POINT ( 'NONE',  ( -0.1144950937579609779, 0.2764156081756484196, 0.4181944444444490316 ) ) ;
#17543 = EDGE_LOOP ( 'NONE', ( #9287, #1276, #4441, #14672 ) ) ;
#17544 = CARTESIAN_POINT ( 'NONE',  ( -0.06071790806472386615, 5.116734183609173314, 0.3033984148421727811 ) ) ;
#17545 = DIRECTION ( 'NONE',  ( -0.000000000000000000, -1.000000000000000000, -0.000000000000000000 ) ) ;
#17546 = DIRECTION ( 'NONE',  ( 0.000000000000000000, 0.000000000000000000, -1.000000000000000000 ) ) ;
#17547 = CARTESIAN_POINT ( 'NONE',  ( -0.1292346314604056190, 0.4798611111111107386, -0.3119999999999999996 ) ) ;
#17548 = CARTESIAN_POINT ( 'NONE',  ( -0.3119999999999998885, 4.887583333333331836, 0.1292346314604058410 ) ) ;
#17549 = CARTESIAN_POINT ( 'NONE',  ( -0.1993543840281266910, 4.082027777853643791, -0.1993543840281266910 ) ) ;
#17550 = CARTESIAN_POINT ( 'NONE',  ( -0.1292346314604058410, 0.6048611109593781121, 0.3119999999999998885 ) ) ;
#17551 = CARTESIAN_POINT ( 'NONE',  ( -0.08099032061185373887, 0.4945060939582657245, 0.4113389257669837762 ) ) ;
#17552 = CARTESIAN_POINT ( 'NONE',  ( 0.1891708636127259202, 2.539511724522405989E-17, 0.3078630284654709781 ) ) ;
#17553 = ORIENTED_EDGE ( 'NONE', *, *, #19139, .T. ) ;
#17554 = ORIENTED_EDGE ( 'NONE', *, *, #5096, .F. ) ;
#17555 = CARTESIAN_POINT ( 'NONE',  ( -0.2209708691207961373, -0.2209708691207961095, -0.03666666666666560520 ) ) ;
#17556 = CARTESIAN_POINT ( 'NONE',  ( 0.1167790944451424368, 4.814666666742533074, 0.2819296736111110424 ) ) ;
#17557 = ADVANCED_FACE ( 'NONE', ( #18184 ), #8917, .T. ) ;
#17558 = AXIS2_PLACEMENT_3D ( 'NONE', #17473, #15410, #15169 ) ;
#17559 = CARTESIAN_POINT ( 'NONE',  ( -0.01976297047192629441, 5.166874033658601206, 0.2975431225754354148 ) ) ;
#17560 = CIRCLE ( 'NONE', #7046, 0.2109499999999996100 ) ;
#17561 = DATE_AND_TIME ( #9891, #5648 ) ;
#17562 = CARTESIAN_POINT ( 'NONE',  ( -0.4687500000000003886, -0.1743457508753611940, 0.07807959546537707185 ) ) ;
#17563 = CARTESIAN_POINT ( 'NONE',  ( -3.385114897866767815E-17, -0.2764156081756484196, 0.04666666666666822311 ) ) ;
#17564 = CARTESIAN_POINT ( 'NONE',  ( 0.1167790944451422702, 4.404944444520309865, -0.2819296736111110979 ) ) ;
#17565 = PERSON_AND_ORGANIZATION_ROLE ( 'classification_officer' ) ;
#17566 = DIRECTION ( 'NONE',  ( -0.7745966692414836263, -0.4472135954999552077, -0.4472135954999600926 ) ) ;
#17567 = CARTESIAN_POINT ( 'NONE',  ( 0.03174294256098305483, 2.685901063997346405, -0.8524985337548631747 ) ) ;
#17568 = CARTESIAN_POINT ( 'NONE',  ( -0.2764156081756484196, 1.692557448933383907E-17, 0.2063888888888917028 ) ) ;
#17569 = CARTESIAN_POINT ( 'NONE',  ( 0.06335377612981493711, 0.2411162243409586958, 0.3999999999999999667 ) ) ;
#17570 = CARTESIAN_POINT ( 'NONE',  ( -0.1993543840281267465, 0.4173611110352444808, 0.1993543840281266633 ) ) ;
#17571 = CARTESIAN_POINT ( 'NONE',  ( -0.4805070082343984583, 0.2560807851245828770, 0.04413116910601658921 ) ) ;
#17572 = CARTESIAN_POINT ( 'NONE',  ( 0.3125000000000000000, 3.827021247335477694E-17, 1.326383476483184332 ) ) ;
#17573 = CARTESIAN_POINT ( 'NONE',  ( 0.000000000000000000, 0.3125000000000000000, -0.008888888888887978151 ) ) ;
#17574 = CARTESIAN_POINT ( 'NONE',  ( -0.3155070326520293400, -0.1306872919485614626, 0.2879861111111143290 ) ) ;
#17575 = CARTESIAN_POINT ( 'NONE',  ( 0.3950000000000000178, 2.665000000000000036, -2.591000000000000192 ) ) ;
#17576 = DIRECTION ( 'NONE',  ( -0.000000000000000000, -1.000000000000000000, -0.000000000000000000 ) ) ;
#17577 = CARTESIAN_POINT ( 'NONE',  ( 1.726321361862525858E-17, 0.3826388888130222710, -0.2819296736111110979 ) ) ;
#17578 = CARTESIAN_POINT ( 'NONE',  ( 0.2819296736111110424, 0.3722222221463555858, -0.1167790944451423119 ) ) ;
#17579 = VECTOR ( 'NONE', #4808, 39.37007874015748854 ) ;
#17580 = CARTESIAN_POINT ( 'NONE',  ( 0.1167790944451424368, 4.050777777853643791, 0.2819296736111110424 ) ) ;
#17581 = CARTESIAN_POINT ( 'NONE',  ( -7.726019084026502927E-17, 0.3017857140906293756, 0.4205848896953069405 ) ) ;
#17582 = CARTESIAN_POINT ( 'NONE',  ( 0.1993543840281266633, 4.734805555631421470, -0.1993543840281266910 ) ) ;
#17583 = CARTESIAN_POINT ( 'NONE',  ( -0.4254287158503465838, 0.3089275304546714174, 0.05347130368200839201 ) ) ;
#17584 = CARTESIAN_POINT ( 'NONE',  ( 0.3119999999999999996, 0.4034722220704893281, -0.1292346314604056468 ) ) ;
#17585 = VERTEX_POINT ( 'NONE', #9153 ) ;
#17586 = DIRECTION ( 'NONE',  ( -0.000000000000000000, -1.000000000000000000, -0.000000000000000000 ) ) ;
#17587 = CARTESIAN_POINT ( 'NONE',  ( 0.2206173157302028787, 3.856333333485065573, 0.2206173157302027954 ) ) ;
#17588 = CARTESIAN_POINT ( 'NONE',  ( 0.000000000000000000, 0.8699999999999998845, 0.000000000000000000 ) ) ;
#17589 =( CONVERSION_BASED_UNIT ( 'INCH', #21603 ) LENGTH_UNIT ( ) NAMED_UNIT ( #19586 ) );
#17590 = CARTESIAN_POINT ( 'NONE',  ( 0.1745307416045020210, 0.03242967361111057101, 0.2218791675890348369 ) ) ;
#17591 = CARTESIAN_POINT ( 'NONE',  ( 0.000000000000000000, 0.06786299768266475241, -0.3150000000000000022 ) ) ;
#17592 = SECURITY_CLASSIFICATION_LEVEL ( 'unclassified' ) ;
#17593 = ORIENTED_EDGE ( 'NONE', *, *, #1357, .T. ) ;
#17594 = CARTESIAN_POINT ( 'NONE',  ( 0.000000000000000000, 0.7650000000000000133, 0.000000000000000000 ) ) ;
#17595 = CARTESIAN_POINT ( 'NONE',  ( -0.03821557678642730632, 4.570560848383669494, 0.3097108463167145276 ) ) ;
#17596 = ADVANCED_FACE ( 'NONE', ( #16598 ), #24018, .T. ) ;
#17597 = ORIENTED_EDGE ( 'NONE', *, *, #13849, .F. ) ;
#17598 = CARTESIAN_POINT ( 'NONE',  ( -0.1167790944451422702, 0.01111111103524447911, -0.2819296736111110424 ) ) ;
#17599 = CARTESIAN_POINT ( 'NONE',  ( 0.2755167264257329940, 4.256510519907095613, -0.1465522358712102458 ) ) ;
#17600 = EDGE_CURVE ( 'NONE', #9081, #1635, #16105, .T. ) ;
#17601 = CARTESIAN_POINT ( 'NONE',  ( 1.910449006669871087E-17, 0.3097222222222218435, -0.3119999999999999996 ) ) ;
#17602 = CARTESIAN_POINT ( 'NONE',  ( 0.2933236148087240980, 4.082464510228600574, 0.1065868417401308055 ) ) ;
#17603 = CARTESIAN_POINT ( 'NONE',  ( 0.2923287055106771337, 0.2008928570453147044, 0.2123892367102621359 ) ) ;
#17604 = CARTESIAN_POINT ( 'NONE',  ( 0.2929506655323979580, 5.178423916424801376, 0.02240466457521756924 ) ) ;
#17605 = CARTESIAN_POINT ( 'NONE',  ( 0.3613381517857143232, 0.3723214284738861068, -0.1174058825155740587 ) ) ;
#17606 = CARTESIAN_POINT ( 'NONE',  ( -0.3236067977499790249, 0.1482142855192009057, 0.2351141009169892271 ) ) ;
#17607 = CARTESIAN_POINT ( 'NONE',  ( -0.1167790944451423257, 5.245222222298087544, -0.2819296736111110424 ) ) ;
#17608 = MANIFOLD_SOLID_BREP ( 'Cut-Extrude3', #15800 ) ;
#17609 = CARTESIAN_POINT ( 'NONE',  ( 0.009843460600206053318, 5.016272758367148477, 0.3119999979945484725 ) ) ;
#17610 = CARTESIAN_POINT ( 'NONE',  ( -0.03815311363224990066, 5.163840424806421581, -0.2966550781246561908 ) ) ;
#17611 = CARTESIAN_POINT ( 'NONE',  ( -0.1742279429200807583, 4.788667672295877864, 0.2618698547778107177 ) ) ;
#17612 = CARTESIAN_POINT ( 'NONE',  ( -0.3119999999999999996, 4.443138889040621820, -0.1292346314604056468 ) ) ;
#17613 = CARTESIAN_POINT ( 'NONE',  ( -1.726321361862525858E-17, 4.630638888964754507, -0.2819296736111110979 ) ) ;
#17614 = ORIENTED_EDGE ( 'NONE', *, *, #18374, .F. ) ;
#17615 = CARTESIAN_POINT ( 'NONE',  ( 0.2819296736111110424, 4.161888888964755395, -0.1167790944451423396 ) ) ;
#17616 = ORIENTED_EDGE ( 'NONE', *, *, #9970, .F. ) ;
#17617 = CIRCLE ( 'NONE', #99, 0.3119999999999999996 ) ;
#17618 = ORIENTED_EDGE ( 'NONE', *, *, #12902, .T. ) ;
#17619 = VERTEX_POINT ( 'NONE', #11350 ) ;
#17620 = CALENDAR_DATE ( 2026, 7, 10 ) ;
#17621 = VERTEX_POINT ( 'NONE', #7804 ) ;
#17622 = CARTESIAN_POINT ( 'NONE',  ( 0.4500000000000003442, 0.2598076211353318454, 0.4425000000000000044 ) ) ;
#17623 = PLANE ( 'NONE',  #7720 ) ;
#17624 = EDGE_CURVE ( 'NONE', #21451, #16665, #4633, .T. ) ;
#17625 = CARTESIAN_POINT ( 'NONE',  ( -0.3119999999999999996, 0.03888888873715596467, -3.820898013339742174E-17 ) ) ;
#17626 = DIRECTION ( 'NONE',  ( 0.000000000000000000, 0.000000000000000000, -1.000000000000000000 ) ) ;
#17627 = CARTESIAN_POINT ( 'NONE',  ( 0.3119999999999999996, 0.1777777776260448250, 0.000000000000000000 ) ) ;
#17628 = CARTESIAN_POINT ( 'NONE',  ( -0.4687500000000002776, 0.04392189231563564666, 0.4181471319205499748 ) ) ;
#17629 = CARTESIAN_POINT ( 'NONE',  ( 0.2206173157302028232, 0.2402777776260448528, -0.2206173157302028232 ) ) ;
#17630 = CARTESIAN_POINT ( 'NONE',  ( 0.000000000000000000, 2.735000000000000320, 0.000000000000000000 ) ) ;
#17631 = CARTESIAN_POINT ( 'NONE',  ( 0.1144950937579609085, -0.2764156081756484751, -0.005416666666665539281 ) ) ;
#17632 = DIRECTION ( 'NONE',  ( 0.000000000000000000, 0.000000000000000000, -1.000000000000000000 ) ) ;
#17633 = AXIS2_PLACEMENT_3D ( 'NONE', #19580, #14103, #1174 ) ;
#17634 = EDGE_CURVE ( 'NONE', #18353, #8579, #2074, .T. ) ;
#17635 = CARTESIAN_POINT ( 'NONE',  ( -0.2819296736111110424, 4.349388888964754507, -0.1167790944451423119 ) ) ;
#17636 = CARTESIAN_POINT ( 'NONE',  ( 0.3119999999999999996, 0.1881944444444441367, -0.1292346314604056468 ) ) ;
#17637 = CARTESIAN_POINT ( 'NONE',  ( -0.02060854148827287805, 0.1800000000000000211, -1.243000000000000327 ) ) ;
#17638 = CARTESIAN_POINT ( 'NONE',  ( -0.3125000000000000000, 0.04488961648812229976, -0.1003708124548366720 ) ) ;
#17639 = DIRECTION ( 'NONE',  ( -0.4999999999999942268, 0.000000000000000000, -0.8660254037844420383 ) ) ;
#17640 = CARTESIAN_POINT ( 'NONE',  ( 0.3119999999999999996, 4.241749999999999687, 0.1292346314604056190 ) ) ;
#17641 = CARTESIAN_POINT ( 'NONE',  ( 0.2530624153226711526, 5.072996518863750026, 0.1824922298374807572 ) ) ;
#17642 = CARTESIAN_POINT ( 'NONE',  ( 0.3119169361980965727, 4.974168473823462833, 0.008358547176593882772 ) ) ;
#17643 = CARTESIAN_POINT ( 'NONE',  ( 0.04643773642726162915, 0.5144550377384379258, 0.07051021533369888905 ) ) ;
#17644 = ORIENTED_EDGE ( 'NONE', *, *, #20901, .F. ) ;
#17645 = CARTESIAN_POINT ( 'NONE',  ( 0.07785856030076440670, 4.708349163112260705, -0.3026912953658169037 ) ) ;
#17646 = ORIENTED_EDGE ( 'NONE', *, *, #8703, .T. ) ;
#17647 = VECTOR ( 'NONE', #321, 39.37007874015747433 ) ;
#17648 = CARTESIAN_POINT ( 'NONE',  ( 0.1899549616143030306, 4.132987843917230286, 0.2475100817204148873 ) ) ;
#17649 = CARTESIAN_POINT ( 'NONE',  ( 0.3155070326520292290, 0.1306872919485615736, -0.01409722222222097032 ) ) ;
#17650 = EDGE_CURVE ( 'NONE', #8276, #9492, #18775, .T. ) ;
#17651 = ADVANCED_FACE ( 'NONE', ( #362 ), #18905, .F. ) ;
#17652 = CARTESIAN_POINT ( 'NONE',  ( 0.000000000000000000, 0.9300000000000000488, 0.7700000000000013500 ) ) ;
#17653 = ORIENTED_EDGE ( 'NONE', *, *, #16045, .T. ) ;
#17654 = CARTESIAN_POINT ( 'NONE',  ( 0.3613381517857143232, 0.1330357141881718941, 0.1174058825155742114 ) ) ;
#17655 = CARTESIAN_POINT ( 'NONE',  ( 0.2819296736111110424, 0.5944444443685777957, -0.1167790944451423119 ) ) ;
#17656 = CARTESIAN_POINT ( 'NONE',  ( -0.2764156081756484196, 0.1144950937579609918, 0.03625000000000144079 ) ) ;
#17657 = CARTESIAN_POINT ( 'NONE',  ( 3.061616997868382402E-17, 5.501232050807569607, 0.2499999999999999722 ) ) ;
#17658 = CARTESIAN_POINT ( 'NONE',  ( -0.1762772571227776142, -0.2274112121558196364, -0.07676730507356434308 ) ) ;
#17659 = CARTESIAN_POINT ( 'NONE',  ( -0.1954553509668046918, -0.1954553509668046640, 0.3244444444444481435 ) ) ;
#17660 = ADVANCED_FACE ( 'NONE', ( #13428 ), #2207, .T. ) ;
#17661 = ORIENTED_EDGE ( 'NONE', *, *, #14495, .F. ) ;
#17662 = CARTESIAN_POINT ( 'NONE',  ( -0.1487971286937952997, 4.622748527369191507, 0.2742326603549272157 ) ) ;
#17663 = CARTESIAN_POINT ( 'NONE',  ( 0.1236067977499789861, 0.1285714285714285310, -0.3804226065180614236 ) ) ;
#17664 = DIRECTION ( 'NONE',  ( 0.4999999999999760192, 0.000000000000000000, -0.8660254037844524744 ) ) ;
#17665 = CARTESIAN_POINT ( 'NONE',  ( 0.1292346314604056745, 0.3618055555555552694, -0.3119999999999999996 ) ) ;
#17666 = CARTESIAN_POINT ( 'NONE',  ( 0.2206173157302027954, 5.029944444444443441, -0.2206173157302028232 ) ) ;
#17667 = CARTESIAN_POINT ( 'NONE',  ( -0.1993543840281266355, 4.304250000075865223, 0.1993543840281267465 ) ) ;
#17668 = AXIS2_PLACEMENT_3D ( 'NONE', #19046, #2699, #15750 ) ;
#17669 = CARTESIAN_POINT ( 'NONE',  ( 5.178964085587577574E-17, 4.047305555631421470, 0.2819296736111110979 ) ) ;
#17670 = PLANE ( 'NONE',  #3828 ) ;
#17671 = CARTESIAN_POINT ( 'NONE',  ( -0.4593750000000004219, 0.2760455974562897596, 0.3779506566538943790 ) ) ;
#17672 = CARTESIAN_POINT ( 'NONE',  ( 0.2094516944643866063, 2.389325547265710570E-17, 0.2954011803958429550 ) ) ;
#17673 = ORIENTED_EDGE ( 'NONE', *, *, #2339, .F. ) ;
#17674 = ORIENTED_EDGE ( 'NONE', *, *, #20656, .F. ) ;
#17675 = CARTESIAN_POINT ( 'NONE',  ( 0.3125000000000000000, -5.740531871003217465E-17, -0.01583333333333210996 ) ) ;
#17676 = CARTESIAN_POINT ( 'NONE',  ( 0.2819296736111110979, 4.766055555631421470, 0.1167790944451422425 ) ) ;
#17677 = CARTESIAN_POINT ( 'NONE',  ( 0.3008575146321451621, 0.0004514677251443983508, -0.2006503380323239050 ) ) ;
#17678 = EDGE_CURVE ( 'NONE', #6978, #15714, #15366, .T. ) ;
#17679 = CARTESIAN_POINT ( 'NONE',  ( -0.2060199298796748235, 5.161632575040133730, 0.2171178220200643549 ) ) ;
#17680 = CARTESIAN_POINT ( 'NONE',  ( -0.4795759180132158628, 0.04343035316921608352, 0.07439866462880882769 ) ) ;
#17681 = CARTESIAN_POINT ( 'NONE',  ( 0.000000000000000000, 0.2764156081756484196, 0.07444444444444621445 ) ) ;
#17682 = CARTESIAN_POINT ( 'NONE',  ( 5.178964085587577574E-17, 3.991750000075865223, 0.2819296736111110979 ) ) ;
#17683 = CARTESIAN_POINT ( 'NONE',  ( -0.3109191470435612170, 4.834790615471364461, -0.02595519365989059843 ) ) ;
#17684 = CARTESIAN_POINT ( 'NONE',  ( 0.3247595264191666109, 2.291712385858714285, -0.9871846966950065250 ) ) ;
#17685 = CARTESIAN_POINT ( 'NONE',  ( 0.2764156081756484196, -5.077672346800151106E-17, 0.2341666666666696595 ) ) ;
#17686 = CARTESIAN_POINT ( 'NONE',  ( 3.073863465859856523E-17, 0.4987679491924311148, -0.2510000000000000009 ) ) ;
#17687 = CARTESIAN_POINT ( 'NONE',  ( 0.1167790944451423257, -0.009722222298088854797, -0.2819296736111110424 ) ) ;
#17688 = CARTESIAN_POINT ( 'NONE',  ( 0.05866837512862279475, 0.2818896272181937723, 0.3994403845921892793 ) ) ;
#17689 = CARTESIAN_POINT ( 'NONE',  ( -0.3120000000000000551, 0.4381944444444440534, 0.1292346314604056190 ) ) ;
#17690 = FACE_OUTER_BOUND ( 'NONE', #6869, .T. ) ;
#17691 = CARTESIAN_POINT ( 'NONE',  ( -1.910449006669871087E-17, 3.814666666666665762, -0.3119999999999999996 ) ) ;
#17692 = CARTESIAN_POINT ( 'NONE',  ( 0.000000000000000000, 0.3155070326520292845, 0.4928472222222270993 ) ) ;
#17693 = ORIENTED_EDGE ( 'NONE', *, *, #23606, .F. ) ;
#17694 = FACE_OUTER_BOUND ( 'NONE', #14846, .T. ) ;
#17695 = CARTESIAN_POINT ( 'NONE',  ( 0.000000000000000000, 0.3125000000000000000, 0.3800000000000039457 ) ) ;
#17696 = CARTESIAN_POINT ( 'NONE',  ( 0.2977100099089716734, 3.659999999999999698, 0.09499999999999995948 ) ) ;
#17697 = CARTESIAN_POINT ( 'NONE',  ( -0.2819296736111110979, 0.3999999999241333759, 0.1167790944451422425 ) ) ;
#17698 = CARTESIAN_POINT ( 'NONE',  ( 0.1993543840281267465, 4.054250000075865223, 0.1993543840281266633 ) ) ;
#17699 = CARTESIAN_POINT ( 'NONE',  ( -0.3236067977499790249, 0.4339285712334866041, 0.2351141009169892271 ) ) ;
#17700 = CARTESIAN_POINT ( 'NONE',  ( -1.726321361862525858E-17, 4.741750000075866112, -0.2819296736111110979 ) ) ;
#17701 = CARTESIAN_POINT ( 'NONE',  ( 3.820898013339742174E-17, 5.384999999999999787, 0.3119999999999999996 ) ) ;
#17702 =( BOUNDED_CURVE ( )  B_SPLINE_CURVE ( 2, ( #18584, #7253, #18226, #161, #1522, #16639, #1637, #3581, #5655 ),
 .UNSPECIFIED., .F., .F. ) 
 B_SPLINE_CURVE_WITH_KNOTS ( ( 3, 2, 2, 2, 3 ),
 ( 0.6339285714285713969, 0.6383928571428570953, 0.6428571428571429047, 0.6473214285714286031, 0.6517857142857143016 ),
 .UNSPECIFIED. ) 
 CURVE ( )  GEOMETRIC_REPRESENTATION_ITEM ( )  RATIONAL_B_SPLINE_CURVE ( ( 1.000000000000000000, 0.9238795325112867385, 1.000000000000000000, 0.9238795325112867385, 1.000000000000000000, 0.9238795325112867385, 1.000000000000000000, 0.9238795325112867385, 1.000000000000000000 ) ) 
 REPRESENTATION_ITEM ( '' )  );
#17703 = EDGE_LOOP ( 'NONE', ( #10592, #3197, #12997, #11403 ) ) ;
#17704 = CARTESIAN_POINT ( 'NONE',  ( 0.3125000000000000555, -5.740531871003217465E-17, 0.3730555555555599145 ) ) ;
#17705 = CARTESIAN_POINT ( 'NONE',  ( 0.1292346314604058410, 3.908416666818398610, 0.3119999999999998885 ) ) ;
#17706 = AXIS2_PLACEMENT_3D ( 'NONE', #4805, #2631, #19333 ) ;
#17707 = DIRECTION ( 'NONE',  ( 0.000000000000000000, 0.000000000000000000, 1.000000000000000000 ) ) ;
#17708 = CYLINDRICAL_SURFACE ( 'NONE', #9985, 0.3119999999999999996 ) ;
#17709 = CARTESIAN_POINT ( 'NONE',  ( 0.1770636233842524665, 5.206640035683666845, 0.2200907654775672573 ) ) ;
#17710 = AXIS2_PLACEMENT_3D ( 'NONE', #9645, #1964, #18913 ) ;
#17711 = CARTESIAN_POINT ( 'NONE',  ( 0.2819296736111110979, 4.991750000075866112, -3.452642723725051716E-17 ) ) ;
#17712 = DATE_AND_TIME ( #12005, #15812 ) ;
#17713 = ORIENTED_EDGE ( 'NONE', *, *, #8118, .F. ) ;
#17714 = CARTESIAN_POINT ( 'NONE',  ( 0.3119999999999998885, 0.2368055555555552416, 0.1292346314604058410 ) ) ;
#17715 = ORIENTED_EDGE ( 'NONE', *, *, #20172, .F. ) ;
#17716 = CARTESIAN_POINT ( 'NONE',  ( -0.1993543840281266633, 0.07013888881302225708, -0.1993543840281266910 ) ) ;
#17717 = CARTESIAN_POINT ( 'NONE',  ( -0.1167790944451422702, 0.06666666659080003332, -0.2819296736111110424 ) ) ;
#17718 = EDGE_CURVE ( 'NONE', #7699, #6271, #9759, .T. ) ;
#17719 = CARTESIAN_POINT ( 'NONE',  ( -0.1453203959029216452, 4.733977942634502334, 0.2785166467954151570 ) ) ;
#17720 = CARTESIAN_POINT ( 'NONE',  ( 0.09474597157417177784, 4.074405454342402422, 0.2981878519710033371 ) ) ;
#17721 = AXIS2_PLACEMENT_3D ( 'NONE', #13000, #20771, #4060 ) ;
#17722 = CARTESIAN_POINT ( 'NONE',  ( -0.3613381517857144343, 0.3187499999024576147, 0.1174058825155740171 ) ) ;
#17723 = CARTESIAN_POINT ( 'NONE',  ( -0.3109654920464638983, 5.058820495826127583, 0.03608335268173962912 ) ) ;
#17724 = CARTESIAN_POINT ( 'NONE',  ( -0.02441201398332129568, 4.111524471938507119, -3.542879552481994043 ) ) ;
#17725 = CARTESIAN_POINT ( 'NONE',  ( -0.3308333333333332571, 4.088927411497558688E-17, 0.4425000000000000044 ) ) ;
#17726 = CARTESIAN_POINT ( 'NONE',  ( -1.726321361862525858E-17, 5.241750000075865223, -0.2819296736111110979 ) ) ;
#17727 = CARTESIAN_POINT ( 'NONE',  ( 0.2823059351267606654, 5.033844105951821746, -0.1328440314189146265 ) ) ;
#17728 = APPROVAL_PERSON_ORGANIZATION ( #8523, #14786, #15734 ) ;
#17729 = LINE ( 'NONE', #10544, #16795 ) ;
#17730 = LINE ( 'NONE', #21505, #17910 ) ;
#17731 = CARTESIAN_POINT ( 'NONE',  ( 0.2206173157302028787, 4.523000000151732536, 0.2206173157302027954 ) ) ;
#17732 = CARTESIAN_POINT ( 'NONE',  ( 0.2819296736111111534, 4.613277777853643791, 0.1167790944451422563 ) ) ;
#17733 = ORIENTED_EDGE ( 'NONE', *, *, #13258, .F. ) ;
#17734 = CARTESIAN_POINT ( 'NONE',  ( -0.1993543840281266355, 3.970916666742532186, 0.1993543840281267465 ) ) ;
#17735 = ORIENTED_EDGE ( 'NONE', *, *, #7501, .F. ) ;
#17736 = VECTOR ( 'NONE', #3494, 39.37007874015748143 ) ;
#17737 = VERTEX_POINT ( 'NONE', #18778 ) ;
#17738 = ORIENTED_EDGE ( 'NONE', *, *, #21969, .T. ) ;
#17739 = PERSON_AND_ORGANIZATION ( #15518, #2538 ) ;
#17740 =( BOUNDED_CURVE ( )  B_SPLINE_CURVE ( 2, ( #23213, #19566, #8466, #8599, #23452, #796, #23092, #23328, #6402 ),
 .UNSPECIFIED., .F., .F. ) 
 B_SPLINE_CURVE_WITH_KNOTS ( ( 3, 2, 2, 2, 3 ),
 ( 0.5729166666666667407, 0.5833333333333333703, 0.5937500000000000000, 0.6041666666666667407, 0.6145833333333333703 ),
 .UNSPECIFIED. ) 
 CURVE ( )  GEOMETRIC_REPRESENTATION_ITEM ( )  RATIONAL_B_SPLINE_CURVE ( ( 1.000000000000000000, 0.9238795325112867385, 1.000000000000000000, 0.9238795325112867385, 1.000000000000000000, 0.9238795325112867385, 1.000000000000000000, 0.9238795325112867385, 1.000000000000000000 ) ) 
 REPRESENTATION_ITEM ( '' )  );
#17741 = CC_DESIGN_PERSON_AND_ORGANIZATION_ASSIGNMENT ( #14571, #1400, ( #17744 ) ) ;
#17742 = DIRECTION ( 'NONE',  ( -0.08715574274765827689, 0.9961946980917454342, 0.000000000000000000 ) ) ;
#17743 = CARTESIAN_POINT ( 'NONE',  ( 0.3119999999999999996, 0.4659722222222220100, -0.1292346314604056468 ) ) ;
#17744 = PRODUCT_DEFINITION_FORMATION_WITH_SPECIFIED_SOURCE ( 'ANY', '', #14409, .NOT_KNOWN. ) ;
#17745 = CARTESIAN_POINT ( 'NONE',  ( -0.3119999999999999996, 0.1499999998482670627, -3.820898013339742174E-17 ) ) ;
#17746 = CARTESIAN_POINT ( 'NONE',  ( 0.09752043859265088765, 5.133419670135086044, 0.2908335107427428845 ) ) ;
#17747 = DIRECTION ( 'NONE',  ( -1.000000000000000000, 0.000000000000000000, 0.000000000000000000 ) ) ;
#17748 = CARTESIAN_POINT ( 'NONE',  ( 0.2112257014698199487, 0.3573301435892229927, -0.7196414598378356731 ) ) ;
#17749 = AXIS2_PLACEMENT_3D ( 'NONE', #7572, #9771, #19146 ) ;
#17750 = EDGE_LOOP ( 'NONE', ( #21072, #14520, #18098, #5343, #19981, #9560, #22470, #21763, #15764, #2956, #7999, #5560, #7659, #3972, #8820, #1410 ) ) ;
#17751 = CARTESIAN_POINT ( 'NONE',  ( -0.1954553509668046918, -0.1954553509668046640, 0.3730555555555596925 ) ) ;
#17752 = CARTESIAN_POINT ( 'NONE',  ( -0.2819296736111110979, 0.06319444436857780956, -3.452642723725051716E-17 ) ) ;
#17753 = CARTESIAN_POINT ( 'NONE',  ( 0.1954553509668047195, 0.1954553509668046085, 0.06750000000000172529 ) ) ;
#17754 = DIRECTION ( 'NONE',  ( 0.000000000000000000, 1.000000000000000000, 0.000000000000000000 ) ) ;
#17755 = CONICAL_SURFACE ( 'NONE', #224, 0.3119999999999999996, 0.7853981633974450594 ) ;
#17756 = CARTESIAN_POINT ( 'NONE',  ( 5.178964085587577574E-17, 4.366750000075866112, 0.2819296736111110979 ) ) ;
#17757 = FACE_OUTER_BOUND ( 'NONE', #153, .T. ) ;
#17758 = CARTESIAN_POINT ( 'NONE',  ( -0.3043026786824803431, 0.5532075493895395324, -1.101750068115465941 ) ) ;
#17759 = CARTESIAN_POINT ( 'NONE',  ( -5.731347020009612645E-17, 0.1708333333333330040, 0.3119999999999999996 ) ) ;
#17760 = DIRECTION ( 'NONE',  ( 0.000000000000000000, -0.9961946980917454342, 0.08715574274765833240 ) ) ;
#17761 = CARTESIAN_POINT ( 'NONE',  ( -0.2206173157302027676, 4.335499999999998799, 0.2206173157302028787 ) ) ;
#17762 = CARTESIAN_POINT ( 'NONE',  ( 0.3119999999999999996, 5.144527777929510215, -0.1292346314604056745 ) ) ;
#17763 = CARTESIAN_POINT ( 'NONE',  ( -0.2206173157302027676, 4.668833333333332725, 0.2206173157302028787 ) ) ;
#17764 = LOCAL_TIME ( 21, 9, 13.00000000000000000, #11002 ) ;
#17765 = DIRECTION ( 'NONE',  ( -1.000000000000000000, 0.000000000000000000, 0.000000000000000000 ) ) ;
#17766 = VERTEX_POINT ( 'NONE', #3907 ) ;
#17767 = CARTESIAN_POINT ( 'NONE',  ( -0.1963885513477411360, 4.883221008867676183, -0.2424500834866318566 ) ) ;
#17768 = CIRCLE ( 'NONE', #20105, 0.1874999999999998335 ) ;
#17769 = ADVANCED_FACE ( 'NONE', ( #7682 ), #6369, .F. ) ;
#17770 = CARTESIAN_POINT ( 'NONE',  ( 0.1544305202402338206, 4.131765882334033968, 0.2716318344387808614 ) ) ;
#17771 = CARTESIAN_POINT ( 'NONE',  ( -3.863846776457871776E-17, -0.3155070326520292845, 0.02409722222222379986 ) ) ;
#17772 = DIRECTION ( 'NONE',  ( -1.000000000000000000, 0.000000000000000000, 0.000000000000000000 ) ) ;
#17773 = CARTESIAN_POINT ( 'NONE',  ( 0.000000000000000000, 0.000000000000000000, 0.000000000000000000 ) ) ;
#17774 = CARTESIAN_POINT ( 'NONE',  ( 0.1116596296178199860, 0.1508928570453147155, -0.3436530038418508792 ) ) ;
#17775 = CARTESIAN_POINT ( 'NONE',  ( -0.1167790944451422702, 0.1222222221463555997, -0.2819296736111110979 ) ) ;
#17776 = CARTESIAN_POINT ( 'NONE',  ( -0.2764156081756484196, 1.692557448933383907E-17, -0.07138888888888829387 ) ) ;
#17777 = CARTESIAN_POINT ( 'NONE',  ( 0.08808798601667681971, 1.999640111863030256, -3.163257896446189488 ) ) ;
#17778 = CARTESIAN_POINT ( 'NONE',  ( -0.006674681701965155291, 0.5374122480878897878, 0.05975678175779895046 ) ) ;
#17779 = CARTESIAN_POINT ( 'NONE',  ( -0.2764156081756484196, 0.1144950937579609918, 0.3695833333333374271 ) ) ;
#17780 = ORIENTED_EDGE ( 'NONE', *, *, #5440, .F. ) ;
#17781 = CARTESIAN_POINT ( 'NONE',  ( -0.1920931035936397357, 4.605286123663857367, -0.2458545860066076727 ) ) ;
#17782 = CARTESIAN_POINT ( 'NONE',  ( -0.03359205281520610126, 4.266996909436898022, -0.3104188874939881049 ) ) ;
#17783 = CARTESIAN_POINT ( 'NONE',  ( 0.3450849365154919912, 2.740000000000000213, -1.095874688840917210 ) ) ;
#17784 = CARTESIAN_POINT ( 'NONE',  ( 0.1292346314604057023, 0.3965277777777773682, 0.3119999999999998885 ) ) ;
#17785 = CARTESIAN_POINT ( 'NONE',  ( 5.731347020009612645E-17, 4.897999999999998799, 0.3119999999999999996 ) ) ;
#17786 = VECTOR ( 'NONE', #23638, 39.37007874015748143 ) ;
#17787 = CARTESIAN_POINT ( 'NONE',  ( 0.2819296736111110979, 4.217444444520309865, -0.1167790944451423396 ) ) ;
#17788 = CARTESIAN_POINT ( 'NONE',  ( -0.1993543840281266910, 4.026472222298087544, -0.1993543840281266910 ) ) ;
#17789 = DIRECTION ( 'NONE',  ( -0.8651979924482661177, 0.04370253788966847741, 0.4995222938423191095 ) ) ;
#17790 = DIRECTION ( 'NONE',  ( -0.000000000000000000, -1.000000000000000000, -0.000000000000000000 ) ) ;
#17791 = CARTESIAN_POINT ( 'NONE',  ( 0.3457764953011678855, 1.003480569432279495E-17, 0.1075573247973250213 ) ) ;
#17792 = VERTEX_POINT ( 'NONE', #13555 ) ;
#17793 = EDGE_LOOP ( 'NONE', ( #16871, #17123, #6241, #8619 ) ) ;
#17794 = CARTESIAN_POINT ( 'NONE',  ( 0.3124999999999999445, -0.1294417382415923856, -0.01930555555555435801 ) ) ;
#17795 = CARTESIAN_POINT ( 'NONE',  ( -0.2819296736111110979, 4.408416666742532186, 0.000000000000000000 ) ) ;
#17796 = DIRECTION ( 'NONE',  ( -0.4999999999999916733, 0.000000000000000000, -0.8660254037844433705 ) ) ;
#17797 = CARTESIAN_POINT ( 'NONE',  ( 0.3120000000000000551, 3.797305555555555046, 0.1292346314604056190 ) ) ;
#17798 = ADVANCED_FACE ( 'NONE', ( #2442 ), #9885, .F. ) ;
#17799 = APPLICATION_PROTOCOL_DEFINITION ( 'international standard', 'config_control_design', 1994, #934 ) ;
#17800 = CARTESIAN_POINT ( 'NONE',  ( 0.1988756463526800689, 5.384999999999999787, -0.2404006599154913104 ) ) ;
#17801 = CARTESIAN_POINT ( 'NONE',  ( 0.2764156081756483641, -0.1144950937579611167, 0.001527777777778965927 ) ) ;
#17802 = AXIS2_PLACEMENT_3D ( 'NONE', #15694, #21298, #17883 ) ;
#17803 = CARTESIAN_POINT ( 'NONE',  ( 5.178964085587577574E-17, 4.047305555631421470, 0.2819296736111110979 ) ) ;
#17804 = APPROVAL_ROLE ( '' ) ;
#17805 = CARTESIAN_POINT ( 'NONE',  ( 0.1294417382415924134, 0.3124999999999999445, -0.06791666666666622276 ) ) ;
#17806 = DIRECTION ( 'NONE',  ( 0.4985709748471496283, 0.07555085810113111588, 0.8635502596144277732 ) ) ;
#17807 = CARTESIAN_POINT ( 'NONE',  ( 0.1954553509668047195, 0.1954553509668046085, 0.2411111111111141903 ) ) ;
#17808 = CARTESIAN_POINT ( 'NONE',  ( 0.2923287055106771337, 0.1616071427596004473, -0.2123892367102620249 ) ) ;
#17809 = CARTESIAN_POINT ( 'NONE',  ( 0.1993543840281266355, 0.1395833332574667185, 0.1993543840281267465 ) ) ;
#17810 = CARTESIAN_POINT ( 'NONE',  ( 0.4687500000000002776, -0.08781377892924517592, 0.08855691728830629439 ) ) ;
#17811 = CARTESIAN_POINT ( 'NONE',  ( 0.4795759075923610726, 0.04327673138052716417, 0.07439896364138759433 ) ) ;
#17812 = CARTESIAN_POINT ( 'NONE',  ( -0.3101024306885724058, 0.3622281555308698997, 0.08858850926231193190 ) ) ;
#17813 = CARTESIAN_POINT ( 'NONE',  ( 0.000000000000000000, 0.04999999999999919092, 0.000000000000000000 ) ) ;
#17814 = CARTESIAN_POINT ( 'NONE',  ( -0.3155070326520293400, 0.1306872919485614903, 0.4477083333333378712 ) ) ;
#17815 = EDGE_LOOP ( 'NONE', ( #17948, #7130, #4776, #18880, #4298 ) ) ;
#17816 = CARTESIAN_POINT ( 'NONE',  ( 0.000000000000000000, 2.689999999999999947, 0.000000000000000000 ) ) ;
#17817 = EDGE_CURVE ( 'NONE', #4205, #13263, #8885, .T. ) ;
#17818 = CARTESIAN_POINT ( 'NONE',  ( -0.1917427225863750362, 3.788106276551002072, 0.2494930344764286489 ) ) ;
#17819 = LINE ( 'NONE', #18178, #14819 ) ;
#17820 = CARTESIAN_POINT ( 'NONE',  ( 0.2819296736111110979, 0.3687499999241333759, 0.000000000000000000 ) ) ;
#17821 = CARTESIAN_POINT ( 'NONE',  ( 0.1167790944451422702, 4.071611111186977716, -0.2819296736111110424 ) ) ;
#17822 = CARTESIAN_POINT ( 'NONE',  ( 0.1116596296178199860, 0.09732142847388618179, -0.3436530038418508792 ) ) ;
#17823 = EDGE_LOOP ( 'NONE', ( #6128, #12851, #17378, #2898 ) ) ;
#17824 = CARTESIAN_POINT ( 'NONE',  ( -0.1993543840281266910, 4.582027777853643791, -0.1993543840281266910 ) ) ;
#17825 = CARTESIAN_POINT ( 'NONE',  ( 0.2963689254433287124, 5.132984698410943736, -0.07753672115038566515 ) ) ;
#17826 = CARTESIAN_POINT ( 'NONE',  ( -1.906863420619159052E-17, 5.092106365077719410, -0.3114144293598434809 ) ) ;
#17827 = ADVANCED_FACE ( 'NONE', ( #15607 ), #9085, .F. ) ;
#17828 = ORIENTED_EDGE ( 'NONE', *, *, #12276, .T. ) ;
#17829 = EDGE_CURVE ( 'NONE', #15066, #23116, #23259, .T. ) ;
#17830 = CIRCLE ( 'NONE', #14724, 0.2499999999999999722 ) ;
#17831 = CARTESIAN_POINT ( 'NONE',  ( 0.3119999999999999996, 4.804249999999998799, -0.1292346314604056745 ) ) ;
#17832 = CARTESIAN_POINT ( 'NONE',  ( -0.2206173157302027676, 3.731333333485065129, 0.2206173157302028787 ) ) ;
#17833 = CARTESIAN_POINT ( 'NONE',  ( -0.08311813270112132501, 0.4932776010757430885, 0.4002893343786022018 ) ) ;
#17834 = EDGE_CURVE ( 'NONE', #11818, #16027, #17312, .T. ) ;
#17835 = ORIENTED_EDGE ( 'NONE', *, *, #13344, .T. ) ;
#17836 = CARTESIAN_POINT ( 'NONE',  ( -0.1167790944451423119, 4.786888888964754507, -0.2819296736111110979 ) ) ;
#17837 = PERSON_AND_ORGANIZATION_ROLE ( 'classification_officer' ) ;
#17838 = FACE_OUTER_BOUND ( 'NONE', #847, .T. ) ;
#17839 = CARTESIAN_POINT ( 'NONE',  ( -0.05311512559760463159, 4.570133353518549768, 0.3074461305437241609 ) ) ;
#17840 = ORIENTED_EDGE ( 'NONE', *, *, #10975, .F. ) ;
#17841 = CARTESIAN_POINT ( 'NONE',  ( 0.2819296736111110979, 0.3826388888130222710, 0.000000000000000000 ) ) ;
#17842 = VECTOR ( 'NONE', #15296, 39.37007874015748143 ) ;
#17843 = ORIENTED_EDGE ( 'NONE', *, *, #3498, .T. ) ;
#17844 = CARTESIAN_POINT ( 'NONE',  ( 0.000000000000000000, 5.384999999999999787, 0.000000000000000000 ) ) ;
#17845 = CYLINDRICAL_SURFACE ( 'NONE', #11550, 0.3119999999999999996 ) ;
#17846 = CARTESIAN_POINT ( 'NONE',  ( -0.5116234456863466562, 0.7841300617983542054, 2.630199247266991947 ) ) ;
#17847 = CARTESIAN_POINT ( 'NONE',  ( 0.2233192592356399164, 0.2687499999024575703, 0.3073725909049500604 ) ) ;
#17848 = CARTESIAN_POINT ( 'NONE',  ( -0.3131335442325084983, 5.058051426742139256, 0.009062785932360829452 ) ) ;
#17849 = ADVANCED_FACE ( 'NONE', ( #15956 ), #15725, .T. ) ;
#17850 =( BOUNDED_SURFACE ( )  B_SPLINE_SURFACE ( 3, 2, ( 
 ( #15617, #734, #19621 ),
 ( #10253, #8044, #970 ),
 ( #23388, #15965, #17562 ),
 ( #4627, #6695, #17440 ),
 ( #15496, #14141, #21458 ),
 ( #17680, #4389, #853 ),
 ( #14027, #10016, #15735 ),
 ( #13791, #2568, #23267 ),
 ( #10491, #22923, #2685 ),
 ( #2919, #17920, #8399 ) ),
 .UNSPECIFIED., .F., .F., .F. ) 
 B_SPLINE_SURFACE_WITH_KNOTS ( ( 4, 2, 2, 2, 4 ),
 ( 3, 3 ),
 ( 0.04452332773538494187, 0.04784785823414922090, 0.05117238873291349299, 0.05449691923167777202, 0.05782144973044205105 ),
 ( 0.000000000000000000, 1.000000000000000000 ),
 .UNSPECIFIED. ) 
 GEOMETRIC_REPRESENTATION_ITEM ( )  RATIONAL_B_SPLINE_SURFACE ( (
 ( 1.000000000000000000, 0.8285407536241364834, 1.000000000000000000),
 ( 1.000000000000000000, 0.8326163274272220249, 1.000000000000000000),
 ( 1.000000000000000000, 0.8363775819416653379, 1.000000000000000000),
 ( 1.000000000000000000, 0.8417901505601256273, 1.000000000000000000),
 ( 1.000000000000000000, 0.8433916105626779736, 1.000000000000000000),
 ( 1.000000000000000000, 0.8433912810366652746, 1.000000000000000000),
 ( 1.000000000000000000, 0.8417896183695843249, 1.000000000000000000),
 ( 1.000000000000000000, 0.8363770727355417378, 1.000000000000000000),
 ( 1.000000000000000000, 0.8326160275023869461, 1.000000000000000000),
 ( 1.000000000000000000, 0.8285407536241364834, 1.000000000000000000) ) ) 
 REPRESENTATION_ITEM ( '' )  SURFACE ( )  );
#17851 = CARTESIAN_POINT ( 'NONE',  ( -7.000945310522701902E-17, 0.1678571428571427882, 0.3999999999999999667 ) ) ;
#17852 = ORIENTED_EDGE ( 'NONE', *, *, #6757, .T. ) ;
#17853 = CARTESIAN_POINT ( 'NONE',  ( -1.726321361862525858E-17, 3.783416666742532186, -0.2819296736111110979 ) ) ;
#17854 = CYLINDRICAL_SURFACE ( 'NONE', #10315, 0.7500000000000001110 ) ;
#17855 = CARTESIAN_POINT ( 'NONE',  ( 0.3121171848235045343, 5.031039829910873173, -0.04005612972654293974 ) ) ;
#17856 = FACE_OUTER_BOUND ( 'NONE', #16717, .T. ) ;
#17857 = CARTESIAN_POINT ( 'NONE',  ( 2.936000000000000387, 2.664999999999999591, -2.591000000000000636 ) ) ;
#17858 = CARTESIAN_POINT ( 'NONE',  ( 0.3119999999999999996, 4.474388889040620931, -3.820898013339742174E-17 ) ) ;
#17859 = CARTESIAN_POINT ( 'NONE',  ( -0.2819296736111110979, 4.700083333409199149, 0.000000000000000000 ) ) ;
#17860 = ORIENTED_EDGE ( 'NONE', *, *, #21482, .T. ) ;
#17861 = CARTESIAN_POINT ( 'NONE',  ( -0.1167790944451423535, 4.141055555631421470, 0.2819296736111110424 ) ) ;
#17862 = VECTOR ( 'NONE', #12883, 39.37007874015748143 ) ;
#17863 = EDGE_CURVE ( 'NONE', #4009, #19164, #12628, .T. ) ;
#17864 = EDGE_CURVE ( 'NONE', #23410, #5628, #19256, .T. ) ;
#17865 = DATE_TIME_ROLE ( 'creation_date' ) ;
#17866 = EDGE_LOOP ( 'NONE', ( #1007, #21514, #1874, #16706 ) ) ;
#17867 = CYLINDRICAL_SURFACE ( 'NONE', #9131, 0.3150000000000000577 ) ;
#17868 = DIRECTION ( 'NONE',  ( 0.000000000000000000, 0.000000000000000000, -1.000000000000000000 ) ) ;
#17869 = ORIENTED_EDGE ( 'NONE', *, *, #9220, .T. ) ;
#17870 = CARTESIAN_POINT ( 'NONE',  ( -0.1292346314604056190, 0.3062499998482670627, -0.3119999999999999996 ) ) ;
#17871 = LINE ( 'NONE', #21518, #7788 ) ;
#17872 = CARTESIAN_POINT ( 'NONE',  ( 0.4450000000000002842, 0.000000000000000000, -2.591000000000000192 ) ) ;
#17873 = CARTESIAN_POINT ( 'NONE',  ( 0.06947902941946425270, 0.1664576461568605392, -0.7468889270519576407 ) ) ;
#17874 = AXIS2_PLACEMENT_3D ( 'NONE', #18251, #1308, #17772 ) ;
#17875 = CARTESIAN_POINT ( 'NONE',  ( 0.000000000000000000, 3.738758431839877614E-19, -0.1016666666666665164 ) ) ;
#17876 = CARTESIAN_POINT ( 'NONE',  ( 0.1993543840281266910, 0.04236111103524448085, -0.1993543840281266910 ) ) ;
#17877 = CARTESIAN_POINT ( 'NONE',  ( -0.2764156081756484196, 0.1144950937579609918, -0.02624999999999903799 ) ) ;
#17878 = ORIENTED_EDGE ( 'NONE', *, *, #16175, .F. ) ;
#17879 = CARTESIAN_POINT ( 'NONE',  ( -0.2819296736111110979, 4.408416666742532186, 0.000000000000000000 ) ) ;
#17880 = CARTESIAN_POINT ( 'NONE',  ( 0.1829869529092248703, 0.2292256185136161140, -0.08186893168610080707 ) ) ;
#17881 = CARTESIAN_POINT ( 'NONE',  ( -0.2675307584405086092, 0.3158328359438148381, -1.176588187136770491 ) ) ;
#17882 = CARTESIAN_POINT ( 'NONE',  ( 0.1294417382415921358, -0.3125000000000002220, -0.03319444444444371450 ) ) ;
#17883 = DIRECTION ( 'NONE',  ( -0.8660254037844385966, -0.5000000000000001110, 0.000000000000000000 ) ) ;
#17884 = CARTESIAN_POINT ( 'NONE',  ( -0.1292346314604057023, 4.061194444444443441, 0.3119999999999998885 ) ) ;
#17885 = CARTESIAN_POINT ( 'NONE',  ( -1.910449006669871087E-17, 5.099388889040620931, -0.3119999999999999996 ) ) ;
#17886 = CARTESIAN_POINT ( 'NONE',  ( -0.2206173157302028232, 4.654944444444443441, -0.2206173157302028232 ) ) ;
#17887 = DIMENSIONAL_EXPONENTS ( 1.000000000000000000, 0.000000000000000000, 0.000000000000000000, 0.000000000000000000, 0.000000000000000000, 0.000000000000000000, 0.000000000000000000 ) ;
#17888 = CARTESIAN_POINT ( 'NONE',  ( 0.3850752722190822208, 0.3189425652913191467, 0.07813238993955246015 ) ) ;
#17889 = ORIENTED_EDGE ( 'NONE', *, *, #24055, .F. ) ;
#17890 =( BOUNDED_CURVE ( )  B_SPLINE_CURVE ( 2, ( #299, #20665, #16885, #536, #9819, #15538, #3844, #7973, #15424 ),
 .UNSPECIFIED., .F., .T. ) 
 B_SPLINE_CURVE_WITH_KNOTS ( ( 3, 2, 2, 2, 3 ),
 ( 0.7767857142857145236, 0.7812500000000001110, 0.7857142857142858094, 0.7901785714285713969, 0.7946428571428569843 ),
 .UNSPECIFIED. ) 
 CURVE ( )  GEOMETRIC_REPRESENTATION_ITEM ( )  RATIONAL_B_SPLINE_CURVE ( ( 0.9999999999999962252, 0.9238795325112905132, 1.000000000000000000, 0.9238795325112867385, 1.000000000000000000, 0.9238795325112867385, 1.000000000000000000, 0.9238795325112886259, 0.9999999999999981126 ) ) 
 REPRESENTATION_ITEM ( '' )  );
#17891 = CARTESIAN_POINT ( 'NONE',  ( -0.2498007881920322748, 4.885330436945963584, -0.1913351078665916638 ) ) ;
#17892 = AXIS2_PLACEMENT_3D ( 'NONE', #1481, #20375, #7448 ) ;
#17893 = CARTESIAN_POINT ( 'NONE',  ( -0.3155070326520293400, -0.1306872919485614626, 0.06923611111111301064 ) ) ;
#17894 = CYLINDRICAL_SURFACE ( 'NONE', #11268, 0.3119999999999999996 ) ;
#17895 = B_SPLINE_CURVE_WITH_KNOTS ( 'NONE', 3,
 ( #19551, #14189, #8208, #19797, #22963, #21624, #19671, #4432, #2617, #1020 ),
 .UNSPECIFIED., .F., .F.,
 ( 4, 2, 2, 2, 4 ),
 ( 0.000000000000000000, 0.003270554913819859362, 0.006541109827639718724, 0.009811664741459578953, 0.01308221965527943745 ),
 .UNSPECIFIED. ) ;
#17896 = FACE_OUTER_BOUND ( 'NONE', #22889, .T. ) ;
#17897 = CARTESIAN_POINT ( 'NONE',  ( -6.979263641208234666E-17, 0.2616071427596003973, 0.3799334167787516425 ) ) ;
#17898 = CARTESIAN_POINT ( 'NONE',  ( -0.1993543840281266633, 0.07013888881302225708, -0.1993543840281266910 ) ) ;
#17899 = CARTESIAN_POINT ( 'NONE',  ( 0.1954553509668046640, -0.1954553509668047195, 0.005000000000001192726 ) ) ;
#17900 = FACE_OUTER_BOUND ( 'NONE', #22366, .T. ) ;
#17901 = ADVANCED_FACE ( 'NONE', ( #4733 ), #2085, .F. ) ;
#17902 = CARTESIAN_POINT ( 'NONE',  ( -1.726321361862525858E-17, 5.075083333409198261, -0.2819296736111110979 ) ) ;
#17903 = CARTESIAN_POINT ( 'NONE',  ( 0.2764156081756483641, 0.1144950937579610056, 0.4043055555555599145 ) ) ;
#17904 = VERTEX_POINT ( 'NONE', #6329 ) ;
#17905 = CARTESIAN_POINT ( 'NONE',  ( 0.2206173157302028787, 3.849388888888888083, 0.2206173157302027954 ) ) ;
#17906 = CARTESIAN_POINT ( 'NONE',  ( -0.03916966384476119195, 4.292719081527837766, 0.3096853047877550780 ) ) ;
#17907 = FACE_OUTER_BOUND ( 'NONE', #77, .T. ) ;
#17908 = CARTESIAN_POINT ( 'NONE',  ( -0.1292346314604056190, 0.4243055555555552139, -0.3119999999999999996 ) ) ;
#17909 = CARTESIAN_POINT ( 'NONE',  ( -0.1292346314604057023, 4.616749999999998799, 0.3119999999999998885 ) ) ;
#17910 = VECTOR ( 'NONE', #10545, 39.37007874015748854 ) ;
#17911 = CC_DESIGN_PERSON_AND_ORGANIZATION_ASSIGNMENT ( #13471, #13118, ( #4115 ) ) ;
#17912 = CARTESIAN_POINT ( 'NONE',  ( 0.2819296736111110979, 4.213972222298087544, -3.452642723725051716E-17 ) ) ;
#17913 = CARTESIAN_POINT ( 'NONE',  ( 0.2819296736111110424, 3.898000000075866112, -0.1167790944451423396 ) ) ;
#17914 = CARTESIAN_POINT ( 'NONE',  ( 2.586000000000000298, 0.000000000000000000, -2.591000000000000636 ) ) ;
#17915 = DIRECTION ( 'NONE',  ( -3.642463991552355691E-15, 0.2773500981126160725, 0.9607689228305223983 ) ) ;
#17916 = CARTESIAN_POINT ( 'NONE',  ( 0.03174294256098304789, 2.685901063997346405, -0.8524985337548631747 ) ) ;
#17917 = CARTESIAN_POINT ( 'NONE',  ( -0.1993543840281266355, 4.582027777853642903, 0.1993543840281267465 ) ) ;
#17918 = CARTESIAN_POINT ( 'NONE',  ( -0.2472039951646029798, 4.507996249098253472, 0.1903866923103891273 ) ) ;
#17919 = COORDINATED_UNIVERSAL_TIME_OFFSET ( 0, 0, .AHEAD. ) ;
#17920 = CARTESIAN_POINT ( 'NONE',  ( -0.4687500000000003331, 0.2570931668155772010, 0.04874733047934005220 ) ) ;
#17921 = AXIS2_PLACEMENT_3D ( 'NONE', #17844, #12369, #23546 ) ;
#17922 = CARTESIAN_POINT ( 'NONE',  ( -0.1954553509668046640, 0.1954553509668046918, -0.02972222222222128257 ) ) ;
#17923 = CARTESIAN_POINT ( 'NONE',  ( -0.2819296736111110979, 4.033416666742532186, 0.000000000000000000 ) ) ;
#17924 = CARTESIAN_POINT ( 'NONE',  ( -0.3018196487929861171, 4.837821592016447347, 0.08216582023643356769 ) ) ;
#17925 = DIRECTION ( 'NONE',  ( -0.000000000000000000, -1.000000000000000000, -0.000000000000000000 ) ) ;
#17926 = CARTESIAN_POINT ( 'NONE',  ( 0.000000000000000000, 0.2764156081756484196, 0.1369444444444467002 ) ) ;
#17927 = CARTESIAN_POINT ( 'NONE',  ( -0.2923287055106771337, 0.05446428561674330343, 0.2123892367102619971 ) ) ;
#17928 = CARTESIAN_POINT ( 'NONE',  ( -0.1993543840281267465, 0.01458333325746670114, 0.1993543840281266633 ) ) ;
#17929 = CARTESIAN_POINT ( 'NONE',  ( -0.2977072594216396695, 1.822931211668208286E-17, 0.4093739260883065278 ) ) ;
#17930 = DIRECTION ( 'NONE',  ( -0.000000000000000000, 1.000000000000000000, -0.000000000000000000 ) ) ;
#17931 = SHAPE_REPRESENTATION ( 'Aloris-BXA-Wedge-L', ( #9127 ), #2138 ) ;
#17932 = EDGE_CURVE ( 'NONE', #18090, #18008, #6568, .T. ) ;
#17933 = CARTESIAN_POINT ( 'NONE',  ( -0.04900341404797774192, 0.5861343809992684006, -0.7484292681947780634 ) ) ;
#17934 = CARTESIAN_POINT ( 'NONE',  ( 0.000000000000000000, 0.2764156081756484196, -0.03666666666666578561 ) ) ;
#17935 = CARTESIAN_POINT ( 'NONE',  ( 0.000000000000000000, 0.3155070326520292845, 0.3261805555555591374 ) ) ;
#17936 = ORIENTED_EDGE ( 'NONE', *, *, #294, .T. ) ;
#17937 = CARTESIAN_POINT ( 'NONE',  ( -0.3236067977499789694, 0.07142857142857138297, -0.2351141009169893104 ) ) ;
#17938 = DIRECTION ( 'NONE',  ( 0.000000000000000000, 0.000000000000000000, 1.000000000000000000 ) ) ;
#17939 = CARTESIAN_POINT ( 'NONE',  ( -0.1993543840281266633, 0.5006944443685777957, -0.1993543840281266910 ) ) ;
#17940 = CARTESIAN_POINT ( 'NONE',  ( -0.2819296736111110979, 3.977861111186976828, 0.000000000000000000 ) ) ;
#17941 = CARTESIAN_POINT ( 'NONE',  ( -0.1116596296178199582, 0.03303571418817188854, -0.3436530038418508792 ) ) ;
#17942 = EDGE_CURVE ( 'NONE', #18493, #19908, #18476, .T. ) ;
#17943 = CARTESIAN_POINT ( 'NONE',  ( 0.1993543840281267465, 4.720916666742533074, 0.1993543840281266633 ) ) ;
#17944 = CARTESIAN_POINT ( 'NONE',  ( 0.1265266518300305620, 5.140004865470651829, -0.2773898234840398436 ) ) ;
#17945 = TOROIDAL_SURFACE ( 'NONE', #23053, -0.5601250000000235207, 1.200750000000023521 ) ;
#17946 = CARTESIAN_POINT ( 'NONE',  ( 0.06335377612981431261, 0.1928123468925278527, -0.4000000000000000777 ) ) ;
#17947 = AXIS2_PLACEMENT_3D ( 'NONE', #13662, #4367, #11954 ) ;
#17948 = ORIENTED_EDGE ( 'NONE', *, *, #23175, .F. ) ;
#17949 = CARTESIAN_POINT ( 'NONE',  ( 0.3950000000000000733, 0.04999999999999919092, -0.2605837454876624437 ) ) ;
#17950 = CARTESIAN_POINT ( 'NONE',  ( -0.2819296736111110979, 5.186194444520309865, 0.000000000000000000 ) ) ;
#17951 = LINE ( 'NONE', #14416, #13816 ) ;
#17952 = CARTESIAN_POINT ( 'NONE',  ( 0.05766389498127402063, 0.03242967361111055019, 0.2763512717206497160 ) ) ;
#17953 = CARTESIAN_POINT ( 'NONE',  ( 0.1993543840281267465, 4.873694444520309865, 0.1993543840281266633 ) ) ;
#17954 = APPROVAL_ROLE ( '' ) ;
#17955 = EDGE_LOOP ( 'NONE', ( #5891, #20021, #18819, #18705, #2543 ) ) ;
#17956 = CARTESIAN_POINT ( 'NONE',  ( -0.2992172847943166403, 5.112391783004748724, -0.08165418766530285755 ) ) ;
#17957 = CARTESIAN_POINT ( 'NONE',  ( -0.3119999999999999996, 0.2020833331816004053, -0.1292346314604056745 ) ) ;
#17958 = ORIENTED_EDGE ( 'NONE', *, *, #10876, .T. ) ;
#17959 = CARTESIAN_POINT ( 'NONE',  ( -0.2819296736111110979, 0.3548611110352444808, -3.452642723725051716E-17 ) ) ;
#17960 = EDGE_CURVE ( 'NONE', #14458, #10504, #3075, .T. ) ;
#17961 = AXIS2_PLACEMENT_3D ( 'NONE', #6449, #8273, #17915 ) ;
#17962 = EDGE_CURVE ( 'NONE', #23184, #6211, #12226, .T. ) ;
#17963 = ORIENTED_EDGE ( 'NONE', *, *, #538, .T. ) ;
#17964 = CARTESIAN_POINT ( 'NONE',  ( -0.1993543840281266633, 0.01458333325746670114, -0.1993543840281266910 ) ) ;
#17965 = LINE ( 'NONE', #12251, #4540 ) ;
#17966 = CARTESIAN_POINT ( 'NONE',  ( 0.3017093057370441866, 4.083250499197780492, 0.07947025837465231113 ) ) ;
#17967 = CARTESIAN_POINT ( 'NONE',  ( -0.3236067977499789694, 0.07142857142857138297, -0.2351141009169893104 ) ) ;
#17968 = FACE_OUTER_BOUND ( 'NONE', #12838, .T. ) ;
#17969 = FACE_OUTER_BOUND ( 'NONE', #4324, .T. ) ;
#17970 = CARTESIAN_POINT ( 'NONE',  ( 1.573500000000000343, 0.02500000000000021302, -0.3524999999999999800 ) ) ;
#17971 = CARTESIAN_POINT ( 'NONE',  ( 5.178964085587577574E-17, 4.825083333409199149, 0.2819296736111110979 ) ) ;
#17972 = VERTEX_POINT ( 'NONE', #13623 ) ;
#17973 = CARTESIAN_POINT ( 'NONE',  ( -0.06335377612981472895, 0.1250447955744454220, -0.3999999999999999667 ) ) ;
#17974 = EDGE_CURVE ( 'NONE', #21116, #17172, #3357, .T. ) ;
#17975 = CARTESIAN_POINT ( 'NONE',  ( 0.1993543840281266633, 3.832027777853643791, -0.1993543840281266910 ) ) ;
#17976 = DIRECTION ( 'NONE',  ( 0.4999999999999912292, 0.000000000000000000, -0.8660254037844437036 ) ) ;
#17977 = CARTESIAN_POINT ( 'NONE',  ( 0.2666101000349533900, 5.034820359779531351, -0.1625958559946468762 ) ) ;
#17978 = CARTESIAN_POINT ( 'NONE',  ( -0.4805453480892168949, -0.2624482906435731677, 0.04271891838947986658 ) ) ;
#17979 = CARTESIAN_POINT ( 'NONE',  ( -0.4000000000000000222, 0.2124999998049151573, -4.898587196589413075E-17 ) ) ;
#17980 = CARTESIAN_POINT ( 'NONE',  ( 0.2206173157302028787, 4.189666666818398610, 0.2206173157302027954 ) ) ;
#17981 = CARTESIAN_POINT ( 'NONE',  ( 0.1167790944451424506, 4.661888888964753619, 0.2819296736111110424 ) ) ;
#17982 = ORIENTED_EDGE ( 'NONE', *, *, #7239, .T. ) ;
#17983 = CARTESIAN_POINT ( 'NONE',  ( -0.2819296736111110424, 3.911888888964754507, 0.1167790944451424923 ) ) ;
#17984 = ORIENTED_EDGE ( 'NONE', *, *, #2481, .T. ) ;
#17985 = ORIENTED_EDGE ( 'NONE', *, *, #16283, .T. ) ;
#17986 = ADVANCED_FACE ( 'NONE', ( #13856 ), #10564, .T. ) ;
#17987 = ORIENTED_EDGE ( 'NONE', *, *, #10068, .T. ) ;
#17988 = CALENDAR_DATE ( 2026, 7, 10 ) ;
#17989 = CARTESIAN_POINT ( 'NONE',  ( 0.3120000000000000551, 4.241749999999999687, 0.1292346314604056190 ) ) ;
#17990 = CARTESIAN_POINT ( 'NONE',  ( 2.973500000000002252, 2.702500000000001013, -2.553499999999999215 ) ) ;
#17991 = ORIENTED_EDGE ( 'NONE', *, *, #20167, .F. ) ;
#17992 = CARTESIAN_POINT ( 'NONE',  ( -0.3119999999999999996, 0.3166666665149337478, -3.820898013339742174E-17 ) ) ;
#17993 = CARTESIAN_POINT ( 'NONE',  ( -0.1441205229031398416, 4.381327590240017500, -0.2776377754592725955 ) ) ;
#17994 = CARTESIAN_POINT ( 'NONE',  ( 0.3119999999999998885, 0.1743055554038226151, 0.1292346314604058410 ) ) ;
#17995 = CARTESIAN_POINT ( 'NONE',  ( 0.09469217842228347393, 0.5681098745337339606, -0.7441083818505032088 ) ) ;
#17996 = ORIENTED_EDGE ( 'NONE', *, *, #17634, .T. ) ;
#17997 = ORIENTED_EDGE ( 'NONE', *, *, #8392, .T. ) ;
#17998 = CARTESIAN_POINT ( 'NONE',  ( 0.2206173157302027676, 0.2263888887371559577, 0.2206173157302028787 ) ) ;
#17999 = FACE_OUTER_BOUND ( 'NONE', #1433, .T. ) ;
#18000 = CARTESIAN_POINT ( 'NONE',  ( -0.1954553509668046640, 0.1954553509668046918, 0.1369444444444467002 ) ) ;
#18001 = EDGE_CURVE ( 'NONE', #2257, #15814, #1306, .T. ) ;
#18002 = CARTESIAN_POINT ( 'NONE',  ( 0.2819296736111110979, 4.488277777853643791, 0.1167790944451422425 ) ) ;
#18003 = CARTESIAN_POINT ( 'NONE',  ( 0.2977072594216367274, -5.468793635004571549E-17, -0.08687392608830331320 ) ) ;
#18004 = CARTESIAN_POINT ( 'NONE',  ( -0.2998642343065030524, 0.08796414601291395463, -0.1016666666666771329 ) ) ;
#18005 = CARTESIAN_POINT ( 'NONE',  ( -0.08153216764024100172, 4.212811476589685356, -0.3039061551226592273 ) ) ;
#18006 = CARTESIAN_POINT ( 'NONE',  ( -0.1292346314604056745, 4.151472222222222008, -0.3119999999999999996 ) ) ;
#18007 = CARTESIAN_POINT ( 'NONE',  ( 0.3119999999999999996, 4.918833333485065573, -3.820898013339742174E-17 ) ) ;
#18008 = VERTEX_POINT ( 'NONE', #740 ) ;
#18009 = DIRECTION ( 'NONE',  ( 0.000000000000000000, -1.000000000000000000, 0.000000000000000000 ) ) ;
#18010 = ORIENTED_EDGE ( 'NONE', *, *, #21983, .F. ) ;
#18011 = DIRECTION ( 'NONE',  ( -0.3535533905932763399, -0.7071067811865430208, 0.6123724356957982451 ) ) ;
#18012 = CARTESIAN_POINT ( 'NONE',  ( 0.1306872919485616846, 0.3155070326520292290, 0.04840277777777952234 ) ) ;
#18013 = CARTESIAN_POINT ( 'NONE',  ( 0.000000000000000000, 3.738758431839877614E-19, 0.4241666666666665253 ) ) ;
#18014 = CARTESIAN_POINT ( 'NONE',  ( 0.1116596296178199860, 0.2937499999024575925, -0.3436530038418508792 ) ) ;
#18015 = DIRECTION ( 'NONE',  ( 0.000000000000000000, 1.000000000000000000, 0.000000000000000000 ) ) ;
#18016 = CARTESIAN_POINT ( 'NONE',  ( -0.1954553509668046918, -0.1954553509668046640, 0.04666666666666818841 ) ) ;
#18017 = CARTESIAN_POINT ( 'NONE',  ( -0.1167790944451423257, 5.189666666742533074, -0.2819296736111110424 ) ) ;
#18018 = CARTESIAN_POINT ( 'NONE',  ( 0.1954553509668046640, -0.1954553509668047195, 0.3383333333333371495 ) ) ;
#18019 = VERTEX_POINT ( 'NONE', #15623 ) ;
#18020 = ADVANCED_FACE ( 'NONE', ( #22811 ), #15321, .T. ) ;
#18021 = CARTESIAN_POINT ( 'NONE',  ( 0.1292346314604058410, 3.845916666666666206, 0.3119999999999998885 ) ) ;
#18022 = CARTESIAN_POINT ( 'NONE',  ( -0.004324734472469597517, 4.293710590358529977, 0.3119743139031605494 ) ) ;
#18023 = DIRECTION ( 'NONE',  ( -1.000000000000000000, 0.000000000000000000, 0.000000000000000000 ) ) ;
#18024 = CARTESIAN_POINT ( 'NONE',  ( 0.1292346314604057023, 0.4520833333333330040, 0.3119999999999998885 ) ) ;
#18025 = CARTESIAN_POINT ( 'NONE',  ( -0.3119999999999999996, 4.825083333333331836, -0.1292346314604056468 ) ) ;
#18026 = CARTESIAN_POINT ( 'NONE',  ( 0.2819296736111111534, 4.321611111186976828, 0.1167790944451422563 ) ) ;
#18027 = CARTESIAN_POINT ( 'NONE',  ( 1.973001146175422216, 2.291712385858714729, -1.876529041877834203 ) ) ;
#18028 =( BOUNDED_CURVE ( )  B_SPLINE_CURVE ( 2, ( #10271, #16352, #14043, #6714, #7084, #21827, #23281, #14278, #3175 ),
 .UNSPECIFIED., .F., .T. ) 
 B_SPLINE_CURVE_WITH_KNOTS ( ( 3, 2, 2, 2, 3 ),
 ( 0.1875000000000000278, 0.1979166666666666852, 0.2083333333333333981, 0.2187500000000000555, 0.2291666666666667407 ),
 .UNSPECIFIED. ) 
 CURVE ( )  GEOMETRIC_REPRESENTATION_ITEM ( )  RATIONAL_B_SPLINE_CURVE ( ( 0.9999999999999997780, 0.9238795325112869605, 1.000000000000000000, 0.9238795325112867385, 1.000000000000000000, 0.9238795325112867385, 1.000000000000000000, 0.9238795325112861834, 1.000000000000000666 ) ) 
 REPRESENTATION_ITEM ( '' )  );
#18029 = CARTESIAN_POINT ( 'NONE',  ( -5.731347020009612645E-17, 0.3374999999999996336, 0.3119999999999999996 ) ) ;
#18030 = DIRECTION ( 'NONE',  ( -0.8660254037844434816, -0.000000000000000000, -0.4999999999999914513 ) ) ;
#18031 =( BOUNDED_CURVE ( )  B_SPLINE_CURVE ( 2, ( #472, #22425, #9388, #20718, #110, #237, #4130, #11587, #7903 ),
 .UNSPECIFIED., .F., .F. ) 
 B_SPLINE_CURVE_WITH_KNOTS ( ( 3, 2, 2, 2, 3 ),
 ( 0.2708333333333333148, 0.2812500000000000000, 0.2916666666666666852, 0.3020833333333333148, 0.3125000000000000000 ),
 .UNSPECIFIED. ) 
 CURVE ( )  GEOMETRIC_REPRESENTATION_ITEM ( )  RATIONAL_B_SPLINE_CURVE ( ( 1.000000000000000000, 0.9238795325112867385, 1.000000000000000000, 0.9238795325112867385, 1.000000000000000000, 0.9238795325112867385, 1.000000000000000000, 0.9238795325112867385, 1.000000000000000000 ) ) 
 REPRESENTATION_ITEM ( '' )  );
#18032 = CARTESIAN_POINT ( 'NONE',  ( 0.000000000000000000, 3.514980167629567998, 0.000000000000000000 ) ) ;
#18033 = CARTESIAN_POINT ( 'NONE',  ( 0.1993543840281266633, 4.554250000075866112, -0.1993543840281266910 ) ) ;
#18034 = VECTOR ( 'NONE', #9912, 39.37007874015748854 ) ;
#18035 = CARTESIAN_POINT ( 'NONE',  ( -0.2536818300626839662, 4.507685682728529208, 0.1817722763046524526 ) ) ;
#18036 = CALENDAR_DATE ( 2026, 7, 10 ) ;
#18037 = LINE ( 'NONE', #19862, #4136 ) ;
#18038 = CARTESIAN_POINT ( 'NONE',  ( 0.2764156081756484196, -5.077672346800151106E-17, 0.1161111111111132049 ) ) ;
#18039 = CARTESIAN_POINT ( 'NONE',  ( 0.2819296736111110979, 4.120222222298087544, -0.1167790944451423396 ) ) ;
#18040 = CARTESIAN_POINT ( 'NONE',  ( -0.3104648678880025936, 4.836571241263951215, 0.03818230244409723251 ) ) ;
#18041 = CARTESIAN_POINT ( 'NONE',  ( 0.000000000000000000, 5.384999999999999787, 0.000000000000000000 ) ) ;
#18042 = APPROVAL ( #4981, 'UNSPECIFIED' ) ;
#18043 = CARTESIAN_POINT ( 'NONE',  ( 0.1144950937579609085, -0.2764156081756484751, 0.1126388888888909395 ) ) ;
#18044 = CARTESIAN_POINT ( 'NONE',  ( -0.1116596296178200276, 0.1330357141881718386, 0.3436530038418508792 ) ) ;
#18045 = CARTESIAN_POINT ( 'NONE',  ( -5.178964085587577574E-17, 0.07708333325746669074, 0.2819296736111110979 ) ) ;
#18046 = CARTESIAN_POINT ( 'NONE',  ( 0.3125000000000000000, -5.740531871003217465E-17, -0.07138888888888809958 ) ) ;
#18047 = CYLINDRICAL_SURFACE ( 'NONE', #12750, 0.4000000000000000222 ) ;
#18048 = CARTESIAN_POINT ( 'NONE',  ( -0.06335377612981457629, 0.1660266328018982773, 0.3999999999999999667 ) ) ;
#18049 = CARTESIAN_POINT ( 'NONE',  ( 0.1144950937579609085, -0.2764156081756484751, -0.06097222222222153931 ) ) ;
#18050 = CARTESIAN_POINT ( 'NONE',  ( -0.1306872919485614903, 0.3155070326520293400, 0.4407638888888934514 ) ) ;
#18051 = AXIS2_PLACEMENT_3D ( 'NONE', #17686, #22691, #2692 ) ;
#18052 = ORIENTED_EDGE ( 'NONE', *, *, #521, .T. ) ;
#18053 = CARTESIAN_POINT ( 'NONE',  ( -0.1236067977499790416, 0.09285714285714280480, 0.3804226065180614236 ) ) ;
#18054 = CARTESIAN_POINT ( 'NONE',  ( 2.827183371398320766, 0.9578965207785177238, -3.893896520778517889 ) ) ;
#18055 = CARTESIAN_POINT ( 'NONE',  ( -0.2819296736111110979, 0.5076388888130222155, -3.452642723725051716E-17 ) ) ;
#18056 = CARTESIAN_POINT ( 'NONE',  ( 0.1993543840281267465, 3.943138888964754951, 0.1993543840281266633 ) ) ;
#18057 = CARTESIAN_POINT ( 'NONE',  ( 0.1116596296178199027, 0.06874999990245758696, 0.3436530038418508792 ) ) ;
#18058 = CARTESIAN_POINT ( 'NONE',  ( 5.178964085587577574E-17, 4.491750000075866112, 0.2819296736111110979 ) ) ;
#18059 = CARTESIAN_POINT ( 'NONE',  ( 0.1871732423712090254, 5.138164441764971890, -0.2418006535867516238 ) ) ;
#18060 = VERTEX_POINT ( 'NONE', #20980 ) ;
#18061 = CARTESIAN_POINT ( 'NONE',  ( -0.1167790944451423535, 5.196611111186976828, 0.2819296736111110424 ) ) ;
#18062 = DIRECTION ( 'NONE',  ( 0.8660254037844382635, 0.000000000000000000, 0.5000000000000004441 ) ) ;
#18063 = ADVANCED_FACE ( 'NONE', ( #8169 ), #11731, .T. ) ;
#18064 = AXIS2_PLACEMENT_3D ( 'NONE', #16830, #11223, #3899 ) ;
#18065 = SHAPE_REPRESENTATION_RELATIONSHIP ( 'NONE' , 'NONE' ,  #17931, #7396 ) ;
#18066 = FACE_OUTER_BOUND ( 'NONE', #16058, .T. ) ;
#18067 = CARTESIAN_POINT ( 'NONE',  ( -0.1167790944451423119, 4.953555555631421470, -0.2819296736111110979 ) ) ;
#18068 = CALENDAR_DATE ( 2026, 7, 10 ) ;
#18069 = ORIENTED_EDGE ( 'NONE', *, *, #1578, .T. ) ;
#18070 = EDGE_CURVE ( 'NONE', #13860, #7566, #21666, .T. ) ;
#18071 = CARTESIAN_POINT ( 'NONE',  ( -0.01006672540870686382, 5.100353940687614163, -0.3107987198613663127 ) ) ;
#18072 = CARTESIAN_POINT ( 'NONE',  ( 0.1292346314604057300, 0.2298611111111107941, 0.3119999999999998885 ) ) ;
#18073 = ORIENTED_EDGE ( 'NONE', *, *, #4979, .F. ) ;
#18074 = CARTESIAN_POINT ( 'NONE',  ( -5.178964085587577574E-17, 0.3131944443685777957, 0.2819296736111110979 ) ) ;
#18075 = ORIENTED_EDGE ( 'NONE', *, *, #646, .F. ) ;
#18076 = CARTESIAN_POINT ( 'NONE',  ( 0.1993543840281266910, 0.0006944443685778138933, -0.1993543840281266910 ) ) ;
#18077 = CARTESIAN_POINT ( 'NONE',  ( -0.3125000000000000000, 3.738758431839877614E-19, -0.1016666666666665164 ) ) ;
#18078 = CARTESIAN_POINT ( 'NONE',  ( -0.4416234456863467051, 0.7841300617983542054, 2.589784728423718096 ) ) ;
#18079 = CARTESIAN_POINT ( 'NONE',  ( -0.4000000000000000222, 0.01071428571428569704, 0.1299678784931624920 ) ) ;
#18080 = CARTESIAN_POINT ( 'NONE',  ( -0.2291390410192159499, 5.064333695668232771, 0.2117534099777545753 ) ) ;
#18081 = CARTESIAN_POINT ( 'NONE',  ( 0.3950000000000000178, 2.665000000000000036, -1.966000000000000192 ) ) ;
#18082 = DIRECTION ( 'NONE',  ( -0.000000000000000000, -1.000000000000000000, -0.000000000000000000 ) ) ;
#18083 = LINE ( 'NONE', #1261, #2250 ) ;
#18084 = CARTESIAN_POINT ( 'NONE',  ( 0.2819296736111110424, 4.453555555631421470, -0.1167790944451423396 ) ) ;
#18085 = CARTESIAN_POINT ( 'NONE',  ( 0.2899264469942640088, 4.526525690781284972, 0.1173681943709265485 ) ) ;
#18086 = CARTESIAN_POINT ( 'NONE',  ( -0.2819296736111110424, 3.856333333409198705, 0.1167790944451424923 ) ) ;
#18087 = FACE_OUTER_BOUND ( 'NONE', #21386, .T. ) ;
#18088 = CARTESIAN_POINT ( 'NONE',  ( 0.08111133061092308527, 4.930371998486145380, -0.3019672302974793499 ) ) ;
#18089 = DIRECTION ( 'NONE',  ( 0.000000000000000000, -0.9961946980917454342, 0.08715574274765833240 ) ) ;
#18090 = VERTEX_POINT ( 'NONE', #21347 ) ;
#18091 = LINE ( 'NONE', #6751, #5442 ) ;
#18092 = CARTESIAN_POINT ( 'NONE',  ( 0.3119999999999999996, 4.304250000151731648, 0.1292346314604056190 ) ) ;
#18093 = CARTESIAN_POINT ( 'NONE',  ( 0.1167790944451424506, 4.773000000075866112, 0.2819296736111110424 ) ) ;
#18094 = EDGE_CURVE ( 'NONE', #848, #22975, #2459, .T. ) ;
#18095 = EDGE_CURVE ( 'NONE', #16949, #23326, #7142, .T. ) ;
#18096 = CARTESIAN_POINT ( 'NONE',  ( -0.1167790944451423257, 3.731333333409198261, -0.2819296736111110424 ) ) ;
#18097 = EDGE_CURVE ( 'NONE', #8085, #17737, #2484, .T. ) ;
#18098 = ORIENTED_EDGE ( 'NONE', *, *, #9458, .T. ) ;
#18099 = PRODUCT ( 'Aloris-BXA-Wedge-L', 'Aloris-BXA-Wedge-L', '', ( #12157 ) ) ;
#18100 = EDGE_LOOP ( 'NONE', ( #8742, #16438, #15579 ) ) ;
#18101 = ORIENTED_EDGE ( 'NONE', *, *, #20471, .T. ) ;
#18102 = CALENDAR_DATE ( 2026, 7, 10 ) ;
#18103 = CIRCLE ( 'NONE', #11502, 0.2501339745962155581 ) ;
#18104 = EDGE_CURVE ( 'NONE', #16027, #16427, #6465, .T. ) ;
#18105 = CARTESIAN_POINT ( 'NONE',  ( -0.04076013556702704627, 4.959297389055183025, 0.3120000044509055326 ) ) ;
#18106 = FACE_OUTER_BOUND ( 'NONE', #11810, .T. ) ;
#18107 = VERTEX_POINT ( 'NONE', #17447 ) ;
#18108 = CARTESIAN_POINT ( 'NONE',  ( -0.3119999999999999996, 0.3201388887371559577, 0.1292346314604056190 ) ) ;
#18109 = CARTESIAN_POINT ( 'NONE',  ( -0.3119502584613883522, 4.392308377792550900, 0.04130061492316871447 ) ) ;
#18110 = CARTESIAN_POINT ( 'NONE',  ( -0.1802073857353792830, 5.124029362565509338, 0.2497371168007535003 ) ) ;
#18111 = CARTESIAN_POINT ( 'NONE',  ( -0.2527126213443522951, -0.1892291168972398685, -0.1003708124548348124 ) ) ;
#18112 = CARTESIAN_POINT ( 'NONE',  ( 0.1586331323214220657, 0.5141020712338113530, -0.7330949616466568841 ) ) ;
#18113 = CC_DESIGN_SECURITY_CLASSIFICATION ( #11949, ( #24134 ) ) ;
#18114 = EDGE_LOOP ( 'NONE', ( #13945, #4572, #13385, #19313 ) ) ;
#18115 = LOCAL_TIME ( 21, 9, 13.00000000000000000, #8762 ) ;
#18116 = CARTESIAN_POINT ( 'NONE',  ( 0.1569830666613089287, 5.095142424218626509, -0.2688941244208343795 ) ) ;
#18117 = CARTESIAN_POINT ( 'NONE',  ( 0.1993543840281266910, 0.3201388888130222710, -0.1993543840281266910 ) ) ;
#18118 = CARTESIAN_POINT ( 'NONE',  ( -0.2764156081756484196, -0.1144950937579609362, 0.2029166666666694652 ) ) ;
#18119 = EDGE_LOOP ( 'NONE', ( #17055, #19943, #7843, #22863 ) ) ;
#18120 = CARTESIAN_POINT ( 'NONE',  ( 0.1167790944451424368, 4.536888888964754507, 0.2819296736111110424 ) ) ;
#18121 = CARTESIAN_POINT ( 'NONE',  ( 0.1595362993632637172, 0.2449369388610288245, -0.08132661693453716034 ) ) ;
#18122 = CARTESIAN_POINT ( 'NONE',  ( -1.910449006669871087E-17, 4.592444444444443441, -0.3119999999999999996 ) ) ;
#18123 = FACE_OUTER_BOUND ( 'NONE', #14204, .T. ) ;
#18124 = CARTESIAN_POINT ( 'NONE',  ( 0.1292346314604058410, 4.123694444444445217, 0.3119999999999998885 ) ) ;
#18125 = CARTESIAN_POINT ( 'NONE',  ( 0.3119999999999999996, 5.026472222373954857, 0.1292346314604056190 ) ) ;
#18126 = CIRCLE ( 'NONE', #1756, 0.4062499999999997780 ) ;
#18127 = EDGE_CURVE ( 'NONE', #8682, #17172, #4797, .T. ) ;
#18128 = ORIENTED_EDGE ( 'NONE', *, *, #16335, .F. ) ;
#18129 = DIRECTION ( 'NONE',  ( 0.4999999999999991673, 0.8660254037844390407, -9.106159978880873451E-16 ) ) ;
#18130 = CC_DESIGN_SECURITY_CLASSIFICATION ( #2554, ( #4493 ) ) ;
#18131 = CARTESIAN_POINT ( 'NONE',  ( -0.1740286758623957597, 4.882424925759353052, -0.2591414521710017071 ) ) ;
#18132 = EDGE_CURVE ( 'NONE', #18537, #23057, #7929, .T. ) ;
#18133 = CARTESIAN_POINT ( 'NONE',  ( -0.3155070326520292845, 1.931923388228935888E-17, 0.3435416666666707974 ) ) ;
#18134 = CARTESIAN_POINT ( 'NONE',  ( -0.3613381517857144343, 0.3366071427596004084, 0.1174058825155740171 ) ) ;
#18135 = EDGE_LOOP ( 'NONE', ( #12852, #11352, #4844, #3660 ) ) ;
#18136 = CIRCLE ( 'NONE', #4121, 0.3385998376278290256 ) ;
#18137 = CARTESIAN_POINT ( 'NONE',  ( 0.08316635082768832066, -0.4932497623273898180, 0.4003041662012485347 ) ) ;
#18138 = CARTESIAN_POINT ( 'NONE',  ( -6.979263641208234666E-17, 0.1901785713310290005, 0.3799334167787516425 ) ) ;
#18139 = CARTESIAN_POINT ( 'NONE',  ( -0.2819296736111110979, 0.3513888888130222155, -0.1167790944451423396 ) ) ;
#18140 = CARTESIAN_POINT ( 'NONE',  ( 0.2764156081756483641, 0.1144950937579610056, 0.01541666666666794208 ) ) ;
#18141 = CARTESIAN_POINT ( 'NONE',  ( 0.2819296736111110979, 5.116750000075866112, -3.452642723725051716E-17 ) ) ;
#18142 = CARTESIAN_POINT ( 'NONE',  ( 0.3047585109715561513, 4.472512657067983177, 0.06683305890437241104 ) ) ;
#18143 = EDGE_LOOP ( 'NONE', ( #13410, #12893, #2006, #11446 ) ) ;
#18144 = CARTESIAN_POINT ( 'NONE',  ( -0.1901414604034510070, 4.605216824736812598, -0.2473673753929898356 ) ) ;
#18145 = CARTESIAN_POINT ( 'NONE',  ( 0.4000000000000000222, 0.1142857142857142405, 0.000000000000000000 ) ) ;
#18146 = LOCAL_TIME ( 21, 9, 13.00000000000000000, #10168 ) ;
#18147 = DIRECTION ( 'NONE',  ( -1.000000000000000000, 0.000000000000000000, 0.000000000000000000 ) ) ;
#18148 = CARTESIAN_POINT ( 'NONE',  ( -0.4675994362856803477, 0.2849176297964604587, 0.04270874187135767497 ) ) ;
#18149 = CARTESIAN_POINT ( 'NONE',  ( 5.731347020009612645E-17, 4.786888888888888083, 0.3119999999999999996 ) ) ;
#18150 = CARTESIAN_POINT ( 'NONE',  ( -0.2819296736111110424, 4.023000000075866112, 0.1167790944451424923 ) ) ;
#18151 = CARTESIAN_POINT ( 'NONE',  ( -0.1993543840281266910, 3.804250000075865668, -0.1993543840281266910 ) ) ;
#18152 = CARTESIAN_POINT ( 'NONE',  ( -9.626299801968715084E-16, 0.2035714285714284866, -0.4000000000000000222 ) ) ;
#18153 = CARTESIAN_POINT ( 'NONE',  ( 0.3530939849935142982, 0.9548081934128058723, 2.797609033937592304 ) ) ;
#18154 = VECTOR ( 'NONE', #1092, 39.37007874015748143 ) ;
#18155 = CARTESIAN_POINT ( 'NONE',  ( -0.3119999999999999996, 4.547305555555554157, -0.1292346314604056468 ) ) ;
#18156 = CARTESIAN_POINT ( 'NONE',  ( -1.726321361862525858E-17, 4.505638888964754507, -0.2819296736111110979 ) ) ;
#18157 = CARTESIAN_POINT ( 'NONE',  ( -0.3077250951222398334, 4.500723898767198250, -0.05197174156527661210 ) ) ;
#18158 = DATE_AND_TIME ( #18036, #6813 ) ;
#18159 = DIRECTION ( 'NONE',  ( -0.000000000000000000, -0.000000000000000000, -1.000000000000000000 ) ) ;
#18160 = CARTESIAN_POINT ( 'NONE',  ( -0.1144950937579609918, -0.2764156081756484196, 0.2098611111111139960 ) ) ;
#18161 = CARTESIAN_POINT ( 'NONE',  ( -0.1993543840281266910, 4.026472222298087544, -0.1993543840281266910 ) ) ;
#18162 = CARTESIAN_POINT ( 'NONE',  ( -0.2685085545779261063, 4.830739561115536596, -0.1638191573221950137 ) ) ;
#18163 = CARTESIAN_POINT ( 'NONE',  ( -0.2726119996617456520, 4.451313226511029342, 0.1571456554947538165 ) ) ;
#18164 = CARTESIAN_POINT ( 'NONE',  ( 0.3119999999999998885, 0.06466217752329557478, 0.07460622607702992182 ) ) ;
#18165 = CARTESIAN_POINT ( 'NONE',  ( -0.2233192592356399997, 0.05803571418817187605, 0.3073725909049499494 ) ) ;
#18166 = CIRCLE ( 'NONE', #20501, 0.1850000000000000533 ) ;
#18167 = CARTESIAN_POINT ( 'NONE',  ( -0.2819296736111110979, 0.06666666659080003332, 0.1167790944451422425 ) ) ;
#18168 = CARTESIAN_POINT ( 'NONE',  ( 0.01197057051269882245, 0.2890469299669685688, 0.4003459737656249184 ) ) ;
#18169 = CARTESIAN_POINT ( 'NONE',  ( 0.2472135954999579166, 0.02321428551920091607, 0.3402603233408160732 ) ) ;
#18170 = CARTESIAN_POINT ( 'NONE',  ( -0.05603163257930598301, 0.1624274118792091159, -0.7480337429100453184 ) ) ;
#18171 = CARTESIAN_POINT ( 'NONE',  ( 0.6209078282299125284, 1.869379215919938807E-19, -0.01219352927422984872 ) ) ;
#18172 = CARTESIAN_POINT ( 'NONE',  ( 0.1954553509668046640, -0.1954553509668047195, -0.05055555555555479863 ) ) ;
#18173 = ORIENTED_EDGE ( 'NONE', *, *, #17176, .T. ) ;
#18174 = ORIENTED_EDGE ( 'NONE', *, *, #11723, .F. ) ;
#18175 =( BOUNDED_CURVE ( )  B_SPLINE_CURVE ( 2, ( #9481, #24102, #13162, #5455, #22399, #18503, #14613, #16680, #13039, #9361, #5699, #22521, #13278 ),
 .UNSPECIFIED., .F., .T. ) 
 B_SPLINE_CURVE_WITH_KNOTS ( ( 3, 2, 2, 2, 2, 2, 3 ),
 ( 0.1785714285714285754, 0.1857142857142857206, 0.2000000000000000111, 0.2142857142857142738, 0.2285714285714285643, 0.2428571428571428548, 0.2500000000000000000 ),
 .UNSPECIFIED. ) 
 CURVE ( )  GEOMETRIC_REPRESENTATION_ITEM ( )  RATIONAL_B_SPLINE_CURVE ( ( 0.9755282581475768211, 0.9755282581475768211, 1.000000000000000000, 0.9510565162951535312, 1.000000000000000000, 0.9510565162951535312, 1.000000000000000000, 0.9510565162951535312, 1.000000000000000000, 0.9510565162951535312, 1.000000000000000000, 0.9755282581475767101, 0.9755282581475768211 ) ) 
 REPRESENTATION_ITEM ( '' )  );
#18176 = CARTESIAN_POINT ( 'NONE',  ( 0.05482473137696310811, 0.5228958406531273306, 0.05347130368200837119 ) ) ;
#18177 =( BOUNDED_CURVE ( )  B_SPLINE_CURVE ( 2, ( #23137, #11965, #8153, #8514, #12205, #6812, #11837, #15955, #19614 ),
 .UNSPECIFIED., .F., .F. ) 
 B_SPLINE_CURVE_WITH_KNOTS ( ( 3, 2, 2, 2, 3 ),
 ( 0.8839285714285713969, 0.8883928571428570953, 0.8928571428571427937, 0.8973214285714284921, 0.9017857142857141906 ),
 .UNSPECIFIED. ) 
 CURVE ( )  GEOMETRIC_REPRESENTATION_ITEM ( )  RATIONAL_B_SPLINE_CURVE ( ( 1.000000000000000000, 0.9238795325112867385, 1.000000000000000000, 0.9238795325112867385, 1.000000000000000000, 0.9238795325112867385, 1.000000000000000000, 0.9238795325112886259, 0.9999999999999981126 ) ) 
 REPRESENTATION_ITEM ( '' )  );
#18178 = CARTESIAN_POINT ( 'NONE',  ( 0.08808798601667688910, 4.111524471938507119, -3.348023836630494632 ) ) ;
#18179 = CARTESIAN_POINT ( 'NONE',  ( -0.1292346314604056190, 0.09097222222222188515, -0.3119999999999999996 ) ) ;
#18180 = CARTESIAN_POINT ( 'NONE',  ( 0.1167790944451424368, 3.884111111186977272, 0.2819296736111110424 ) ) ;
#18181 = CARTESIAN_POINT ( 'NONE',  ( 0.3613381517857143232, 0.01160714275960046671, 0.000000000000000000 ) ) ;
#18182 = CARTESIAN_POINT ( 'NONE',  ( 0.2819296736111110979, 4.335500000075866112, 0.1167790944451422425 ) ) ;
#18183 = CARTESIAN_POINT ( 'NONE',  ( 0.7919466436700954848, 2.665000000000000036, -2.986000000000000210 ) ) ;
#18184 = FACE_OUTER_BOUND ( 'NONE', #13732, .T. ) ;
#18185 = ORIENTED_EDGE ( 'NONE', *, *, #11721, .T. ) ;
#18186 = CARTESIAN_POINT ( 'NONE',  ( 0.2406838310274923010, 4.369438628241273825, -0.2001145488402920614 ) ) ;
#18187 = CARTESIAN_POINT ( 'NONE',  ( 0.1993543840281267465, 5.207027777853642903, 0.1993543840281266633 ) ) ;
#18188 = CC_DESIGN_PERSON_AND_ORGANIZATION_ASSIGNMENT ( #2987, #6760, ( #18099 ) ) ;
#18189 = CARTESIAN_POINT ( 'NONE',  ( 0.2309108437718781492, 4.203151657608736436, -0.2098260001596312652 ) ) ;
#18190 = SHAPE_REPRESENTATION_RELATIONSHIP ( 'NONE' , 'NONE' ,  #4350, #22505 ) ;
#18191 = CARTESIAN_POINT ( 'NONE',  ( -0.2819296736111110979, 4.904944444520309865, -0.1167790944451422980 ) ) ;
#18192 = CALENDAR_DATE ( 2026, 7, 10 ) ;
#18193 = ORIENTED_EDGE ( 'NONE', *, *, #13057, .T. ) ;
#18194 = CARTESIAN_POINT ( 'NONE',  ( -0.1539433478974299718, 4.067022932034428884, 0.2713770215894354965 ) ) ;
#18195 = DIRECTION ( 'NONE',  ( 0.7071067811865474617, -0.7071067811865474617, -0.000000000000000000 ) ) ;
#18196 = ORIENTED_EDGE ( 'NONE', *, *, #21533, .F. ) ;
#18197 = CARTESIAN_POINT ( 'NONE',  ( -0.1993543840281267465, 0.2506944443685777957, 0.1993543840281266633 ) ) ;
#18198 = ORIENTED_EDGE ( 'NONE', *, *, #1140, .T. ) ;
#18199 = CARTESIAN_POINT ( 'NONE',  ( 0.1993543840281266910, 0.05624999992413336897, -0.1993543840281266910 ) ) ;
#18200 = CARTESIAN_POINT ( 'NONE',  ( -0.01200529352568108395, 4.710829466525995102, -0.3120383712586302649 ) ) ;
#18201 = CARTESIAN_POINT ( 'NONE',  ( -0.3616234456863465785, 3.514980167629567998, 2.635972749958888528 ) ) ;
#18202 = CARTESIAN_POINT ( 'NONE',  ( -0.1116596296178200276, 0.4008928570453146878, 0.3436530038418508792 ) ) ;
#18203 = CARTESIAN_POINT ( 'NONE',  ( -0.3119999999999998885, 4.498694444444443441, 0.1292346314604058410 ) ) ;
#18204 = CARTESIAN_POINT ( 'NONE',  ( -0.2206173157302027676, 3.779944444444443441, 0.2206173157302028787 ) ) ;
#18205 = CARTESIAN_POINT ( 'NONE',  ( -0.02441201398332155936, 1.999640111863030256, -3.358113612297689343 ) ) ;
#18206 = CARTESIAN_POINT ( 'NONE',  ( 0.3247595264191642794, 2.291712385858714729, -0.9871846966950100777 ) ) ;
#18207 = CARTESIAN_POINT ( 'NONE',  ( -0.1993543840281266910, 4.470916666742532186, -0.1993543840281266910 ) ) ;
#18208 = AXIS2_PLACEMENT_3D ( 'NONE', #17724, #19794, #16261 ) ;
#18209 = DIRECTION ( 'NONE',  ( 0.000000000000000000, 0.000000000000000000, -1.000000000000000000 ) ) ;
#18210 = CARTESIAN_POINT ( 'NONE',  ( -1.853979398150703436E-06, 4.543833384706993606, -0.3119999999944916280 ) ) ;
#18211 = EDGE_CURVE ( 'NONE', #4661, #13477, #9630, .T. ) ;
#18212 = CARTESIAN_POINT ( 'NONE',  ( 0.1993543840281266633, 5.123694444520309865, -0.1993543840281266910 ) ) ;
#18213 = CARTESIAN_POINT ( 'NONE',  ( -0.009820766461577611073, 0.04330690836666935273, -0.2928069083666697825 ) ) ;
#18214 = B_SPLINE_CURVE_WITH_KNOTS ( 'NONE', 3,
 ( #20777, #20543, #15177, #8082, #16998, #530, #18955, #17362, #13356, #7731, #22613, #13243, #9445, #7965, #15417, #5663, #3838, #22845, #6134, #4067, #11522, #170, #11280, #18710, #2008, #16879, #7611, #15063, #22485 ),
 .UNSPECIFIED., .F., .F.,
 ( 4, 2, 1, 1, 1, 1, 1, 2, 2, 2, 2, 2, 2, 2, 2, 2, 4 ),
 ( 0.3015379052287556205, 0.3015433052825606808, 0.3015487053363657965, 0.3015595054439759726, 0.3015811056591962691, 0.3016243060896369177, 0.3017107069505182704, 0.3018835086722808647, 0.3022291121158061644, 0.3029203190028567083, 0.3043027327769577961, 0.3056851465510588839, 0.3070675603251599717, 0.3084499740992610040, 0.3098323878733620917, 0.3112148016474631795, 0.3125972154215642673 ),
 .UNSPECIFIED. ) ;
#18215 = CARTESIAN_POINT ( 'NONE',  ( 0.2725341921420746383, 4.914269569154003037, 0.1572748026637361685 ) ) ;
#18216 = CARTESIAN_POINT ( 'NONE',  ( 0.000000000000000000, 4.111524471938507119, -0.2004988538245859597 ) ) ;
#18217 = CARTESIAN_POINT ( 'NONE',  ( -0.2206173157302027676, 4.286888889040620931, 0.2206173157302028787 ) ) ;
#18218 = EDGE_CURVE ( 'NONE', #1526, #4444, #13445, .T. ) ;
#18219 = CARTESIAN_POINT ( 'NONE',  ( -0.2819296736111110424, 4.536888888964754507, 0.1167790944451424923 ) ) ;
#18220 = CARTESIAN_POINT ( 'NONE',  ( -1.726321361862525858E-17, 3.838972222298087544, -0.2819296736111110979 ) ) ;
#18221 = VERTEX_POINT ( 'NONE', #11608 ) ;
#18222 = ORIENTED_EDGE ( 'NONE', *, *, #23996, .F. ) ;
#18223 = CIRCLE ( 'NONE', #4188, 0.4625000000000000777 ) ;
#18224 = ORIENTED_EDGE ( 'NONE', *, *, #11828, .F. ) ;
#18225 = COORDINATED_UNIVERSAL_TIME_OFFSET ( 0, 0, .AHEAD. ) ;
#18226 = CARTESIAN_POINT ( 'NONE',  ( -0.2206173157302027676, 4.279944444444443441, 0.2206173157302028787 ) ) ;
#18227 = CARTESIAN_POINT ( 'NONE',  ( 2.583392422801339445E-17, 0.8699999999999998845, 0.2109499999999998043 ) ) ;
#18228 = CARTESIAN_POINT ( 'NONE',  ( -5.731347020009612645E-17, 0.4486111111111107386, 0.3119999999999999996 ) ) ;
#18229 = ORIENTED_EDGE ( 'NONE', *, *, #17048, .F. ) ;
#18230 = CARTESIAN_POINT ( 'NONE',  ( 0.2206173157302027676, 0.2263888887371559577, 0.2206173157302028787 ) ) ;
#18231 = CARTESIAN_POINT ( 'NONE',  ( -0.001713203249405378893, 4.377212721013385988, -0.3119959714558495079 ) ) ;
#18232 = CARTESIAN_POINT ( 'NONE',  ( -0.2258242712019069010, 5.122164547046700100, 0.2098372851225053237 ) ) ;
#18233 = CARTESIAN_POINT ( 'NONE',  ( 0.1294417382415921358, -0.3125000000000002220, -0.08874999999999971800 ) ) ;
#18234 = CARTESIAN_POINT ( 'NONE',  ( -0.1236067977499790416, 0.3785714285714284477, 0.3804226065180614236 ) ) ;
#18235 = ORIENTED_EDGE ( 'NONE', *, *, #4739, .F. ) ;
#18236 = CARTESIAN_POINT ( 'NONE',  ( 0.2517364957946364168, 5.079917474983905556, 0.1844428286663916672 ) ) ;
#18237 = CARTESIAN_POINT ( 'NONE',  ( 0.2764156081756483641, -0.1144950937579611167, 0.3348611111111149952 ) ) ;
#18238 = CARTESIAN_POINT ( 'NONE',  ( 0.2819296736111110424, 4.161888888964755395, -0.1167790944451423396 ) ) ;
#18239 = CARTESIAN_POINT ( 'NONE',  ( -0.1167790944451423119, 5.175777777853643791, -0.2819296736111110979 ) ) ;
#18240 = CARTESIAN_POINT ( 'NONE',  ( -0.006542161132012624253, -0.5374887588746249945, 0.3892820121258429023 ) ) ;
#18241 = CARTESIAN_POINT ( 'NONE',  ( 0.000000000000000000, 0.3308333333333332571, 0.4425000000000000044 ) ) ;
#18242 = CARTESIAN_POINT ( 'NONE',  ( -0.3119999999999999996, 4.106333333333332725, 0.000000000000000000 ) ) ;
#18243 = CONICAL_SURFACE ( 'NONE', #22895, 0.7199999999999994182, 0.7853981633974506105 ) ;
#18244 = CARTESIAN_POINT ( 'NONE',  ( -0.3119999999999999996, 5.002166666818398610, 0.000000000000000000 ) ) ;
#18245 = ADVANCED_FACE ( 'NONE', ( #2342 ), #8983, .T. ) ;
#18246 = CARTESIAN_POINT ( 'NONE',  ( -0.1993543840281266355, 5.095916666742533074, 0.1993543840281267465 ) ) ;
#18247 = DIRECTION ( 'NONE',  ( 0.5773502691896283956, -0.5773502691896220673, -0.5773502691896265082 ) ) ;
#18248 = ORIENTED_EDGE ( 'NONE', *, *, #11663, .F. ) ;
#18249 = CARTESIAN_POINT ( 'NONE',  ( -0.2137897711831445446, 4.883875763723968255, -0.2274687474526748132 ) ) ;
#18250 = CARTESIAN_POINT ( 'NONE',  ( 0.3155070326520292290, 0.1306872919485615736, 0.1525694444444470055 ) ) ;
#18251 = CARTESIAN_POINT ( 'NONE',  ( 0.000000000000000000, 0.000000000000000000, -0.1199999999999999956 ) ) ;
#18252 = VECTOR ( 'NONE', #4276, 39.37007874015748854 ) ;
#18253 = ORIENTED_EDGE ( 'NONE', *, *, #11988, .T. ) ;
#18254 = CARTESIAN_POINT ( 'NONE',  ( 0.009374999999999975367, -0.5358532185916218271, 0.3779506566538943790 ) ) ;
#18255 = ADVANCED_FACE ( 'NONE', ( #14968 ), #9232, .F. ) ;
#18256 = CARTESIAN_POINT ( 'NONE',  ( 3.827021247335478926E-17, 0.02999999999999995379, 0.3125000000000000000 ) ) ;
#18257 = EDGE_CURVE ( 'NONE', #9037, #13845, #13154, .T. ) ;
#18258 = CARTESIAN_POINT ( 'NONE',  ( 0.1167790944451423535, 0.2055555554796889006, 0.2819296736111110979 ) ) ;
#18259 = CARTESIAN_POINT ( 'NONE',  ( 0.2764156081756483641, 0.1144950937579610056, 0.3487500000000040012 ) ) ;
#18260 = CARTESIAN_POINT ( 'NONE',  ( -1.726321361862525858E-17, 5.186194444520309865, -0.2819296736111110979 ) ) ;
#18261 = CARTESIAN_POINT ( 'NONE',  ( 0.000000000000000000, 5.384999999999999787, -0.3119999999999999996 ) ) ;
#18262 = ORIENTED_EDGE ( 'NONE', *, *, #8264, .T. ) ;
#18263 = CARTESIAN_POINT ( 'NONE',  ( -8.106877718569361257E-06, 3.766055773525306627, -0.3120000000431728537 ) ) ;
#18264 = DIRECTION ( 'NONE',  ( 0.000000000000000000, 0.000000000000000000, -1.000000000000000000 ) ) ;
#18265 = CARTESIAN_POINT ( 'NONE',  ( 0.0003703964654298149100, 4.877156714020134842, -0.3119998122762405734 ) ) ;
#18266 = DIRECTION ( 'NONE',  ( 0.000000000000000000, -1.000000000000000000, 0.000000000000000000 ) ) ;
#18267 = CARTESIAN_POINT ( 'NONE',  ( 0.3119999999999999996, 0.5701388887371559022, -0.1292346314604056468 ) ) ;
#18268 = CARTESIAN_POINT ( 'NONE',  ( -1.910449006669871087E-17, 4.703555555555555046, -0.3119999999999999996 ) ) ;
#18269 = CARTESIAN_POINT ( 'NONE',  ( -0.2819296736111110979, 4.075083333409199149, 0.000000000000000000 ) ) ;
#18270 = CARTESIAN_POINT ( 'NONE',  ( -0.1167790944451423257, 3.856333333409198705, -0.2819296736111110424 ) ) ;
#18271 = EDGE_CURVE ( 'NONE', #21713, #21079, #3376, .T. ) ;
#18272 = CARTESIAN_POINT ( 'NONE',  ( 0.3079291438910055634, 4.028372153496735386, 0.05528882331475011569 ) ) ;
#18273 = DIRECTION ( 'NONE',  ( -1.000000000000000000, 0.000000000000000000, 0.000000000000000000 ) ) ;
#18274 = VECTOR ( 'NONE', #9236, 39.37007874015748143 ) ;
#18275 = CARTESIAN_POINT ( 'NONE',  ( -0.009374999999999905978, -0.5358532185916218271, 0.06112444011295371793 ) ) ;
#18276 = ORIENTED_EDGE ( 'NONE', *, *, #5497, .F. ) ;
#18277 = CARTESIAN_POINT ( 'NONE',  ( 0.1167790944451424368, 4.536888888964754507, 0.2819296736111110424 ) ) ;
#18278 = CARTESIAN_POINT ( 'NONE',  ( -0.3028095456829690835, 4.500036060564890583, -0.07595219160868893482 ) ) ;
#18279 = FACE_OUTER_BOUND ( 'NONE', #18849, .T. ) ;
#18280 = CARTESIAN_POINT ( 'NONE',  ( 0.1954553509668046640, -0.1954553509668047195, 0.3313888888888926743 ) ) ;
#18281 = CARTESIAN_POINT ( 'NONE',  ( 0.2819296736111110979, 3.783416666742532186, -3.452642723725051716E-17 ) ) ;
#18282 = CARTESIAN_POINT ( 'NONE',  ( -0.4581189881604794678, 0.2644951211353315235, 0.3941886329748525153 ) ) ;
#18283 = CARTESIAN_POINT ( 'NONE',  ( 0.000000000000000000, -3.937007874019685528E-05, 0.000000000000000000 ) ) ;
#18284 = DIRECTION ( 'NONE',  ( -0.000000000000000000, -1.000000000000000000, -0.000000000000000000 ) ) ;
#18285 = CARTESIAN_POINT ( 'NONE',  ( -0.3613381517857144343, 0.2651785713310289005, 0.1174058825155740171 ) ) ;
#18286 = AXIS2_PLACEMENT_3D ( 'NONE', #18032, #1687, #9122 ) ;
#18287 = CARTESIAN_POINT ( 'NONE',  ( -0.1167790944451424368, 0.2402777777019111660, 0.2819296736111110424 ) ) ;
#18288 = CARTESIAN_POINT ( 'NONE',  ( 0.3385998376278290256, 4.184039657745742702E-17, -0.1199999999999999956 ) ) ;
#18289 = CARTESIAN_POINT ( 'NONE',  ( 0.3999999999999999667, 0.03035714266205805437, 0.1299678784931626307 ) ) ;
#18290 = CARTESIAN_POINT ( 'NONE',  ( -0.1884161264613055942, 0.4667385597628443406, -0.7259675891464789643 ) ) ;
#18291 = CARTESIAN_POINT ( 'NONE',  ( -0.2764156081756484196, 1.692557448933383907E-17, -0.02277777777777679341 ) ) ;
#18292 = CARTESIAN_POINT ( 'NONE',  ( -0.2764156081756484196, 0.1144950937579609918, -0.01930555555555454883 ) ) ;
#18293 = ORIENTED_EDGE ( 'NONE', *, *, #14666, .T. ) ;
#18294 = ORIENTED_EDGE ( 'NONE', *, *, #10311, .F. ) ;
#18295 = CARTESIAN_POINT ( 'NONE',  ( 0.3143659348029790301, 0.3723832402019556231, 0.07159583130656671512 ) ) ;
#18296 = CARTESIAN_POINT ( 'NONE',  ( -1.910449006669871087E-17, 4.703555555555555046, -0.3119999999999999996 ) ) ;
#18297 = CARTESIAN_POINT ( 'NONE',  ( -0.1292346314604056190, -0.02013888888888922327, -0.3119999999999999996 ) ) ;
#18298 = CARTESIAN_POINT ( 'NONE',  ( -0.2819296736111110424, 3.925777777853644235, 0.1167790944451424923 ) ) ;
#18299 = CARTESIAN_POINT ( 'NONE',  ( 0.2923287055106771337, 0.1616071427596004473, -0.2123892367102620249 ) ) ;
#18300 = CARTESIAN_POINT ( 'NONE',  ( 0.2819296736111110979, 4.391055555631421470, 0.1167790944451422425 ) ) ;
#18301 = EDGE_CURVE ( 'NONE', #2851, #2257, #5326, .T. ) ;
#18302 = DIRECTION ( 'NONE',  ( 0.000000000000000000, 0.000000000000000000, 1.000000000000000000 ) ) ;
#18303 = CARTESIAN_POINT ( 'NONE',  ( -0.3119999999999998885, 4.609805555555555046, 0.1292346314604058410 ) ) ;
#18304 = VERTEX_POINT ( 'NONE', #20326 ) ;
#18305 = CARTESIAN_POINT ( 'NONE',  ( 0.3119999999999999996, 4.689666666666665762, -3.820898013339742174E-17 ) ) ;
#18306 = CARTESIAN_POINT ( 'NONE',  ( 0.2819296736111110424, 5.106333333409198261, -0.1167790944451423396 ) ) ;
#18307 = AXIS2_PLACEMENT_3D ( 'NONE', #4869, #17806, #12451 ) ;
#18308 = CARTESIAN_POINT ( 'NONE',  ( 0.2416695147500300678, 4.202697174923091694, -0.1973961377565022768 ) ) ;
#18309 = AXIS2_PLACEMENT_3D ( 'NONE', #5394, #23793, #7115 ) ;
#18310 =( NAMED_UNIT ( * ) PLANE_ANGLE_UNIT ( ) SI_UNIT ( $, .RADIAN. ) );
#18311 = CARTESIAN_POINT ( 'NONE',  ( 0.000000000000000000, 5.384999999999999787, 0.000000000000000000 ) ) ;
#18312 = CARTESIAN_POINT ( 'NONE',  ( -0.2819296736111110979, 4.627166666742532186, -0.1167790944451422980 ) ) ;
#18313 = APPROVAL_STATUS ( 'not_yet_approved' ) ;
#18314 = CARTESIAN_POINT ( 'NONE',  ( -0.2246295819815997963, 4.064464186035761095, 0.2174240014552116795 ) ) ;
#18315 = CARTESIAN_POINT ( 'NONE',  ( 0.000000000000000000, 2.740000000000000213, 0.000000000000000000 ) ) ;
#18316 = CARTESIAN_POINT ( 'NONE',  ( 0.2819296736111110424, 0.3236111110352444808, 0.1167790944451424923 ) ) ;
#18317 = CARTESIAN_POINT ( 'NONE',  ( -0.2819296736111110979, 0.2472222221463555580, 0.1167790944451422425 ) ) ;
#18318 = PLANE ( 'NONE',  #6097 ) ;
#18319 = CARTESIAN_POINT ( 'NONE',  ( 4.312521114635084752E-13, 5.190332509204934830, -0.2890970118899086061 ) ) ;
#18320 = CARTESIAN_POINT ( 'NONE',  ( -0.3999999999999999667, 0.003571428571428547031, -0.1299678784931626030 ) ) ;
#18321 = FACE_OUTER_BOUND ( 'NONE', #13502, .T. ) ;
#18322 = CARTESIAN_POINT ( 'NONE',  ( -0.3119999999999999996, 3.772999999999999243, 0.000000000000000000 ) ) ;
#18323 = VECTOR ( 'NONE', #18504, 39.37007874015748854 ) ;
#18324 = CARTESIAN_POINT ( 'NONE',  ( -0.007226626051191389552, 3.877360830121420854, -0.3119999924289658666 ) ) ;
#18325 = CARTESIAN_POINT ( 'NONE',  ( 1.036069691232456069, 2.476534978792082509, -1.156303459062617556 ) ) ;
#18326 = VECTOR ( 'NONE', #2312, 39.37007874015748143 ) ;
#18327 = CARTESIAN_POINT ( 'NONE',  ( 0.1993543840281266633, 4.512583333409199149, -0.1993543840281266910 ) ) ;
#18328 = CARTESIAN_POINT ( 'NONE',  ( -0.2472135954999579444, 0.05892857123348662490, -0.3402603233408159622 ) ) ;
#18329 = CARTESIAN_POINT ( 'NONE',  ( 1.910449006669871087E-17, 0.2472222220704892726, -0.3119999999999999996 ) ) ;
#18330 = CARTESIAN_POINT ( 'NONE',  ( -0.1993543840281266355, 4.984805555631421470, 0.1993543840281267465 ) ) ;
#18331 = ADVANCED_FACE ( 'NONE', ( #20449 ), #22029, .T. ) ;
#18332 = PLANE ( 'NONE',  #13830 ) ;
#18333 = CARTESIAN_POINT ( 'NONE',  ( 0.3078657136106562886, 3.750759388707112230, 0.05066613946664001722 ) ) ;
#18334 = CARTESIAN_POINT ( 'NONE',  ( -0.3119999999999999996, 0.4833333331816003775, -3.820898013339742174E-17 ) ) ;
#18335 = CARTESIAN_POINT ( 'NONE',  ( -2.336494862270849996E-07, 3.904935224540334815, 0.3119999999998144258 ) ) ;
#18336 = CARTESIAN_POINT ( 'NONE',  ( 0.2206173157302028787, 4.245222222373954857, 0.2206173157302027954 ) ) ;
#18337 = CARTESIAN_POINT ( 'NONE',  ( 5.178964085587577574E-17, 4.491750000075866112, 0.2819296736111110979 ) ) ;
#18338 = CARTESIAN_POINT ( 'NONE',  ( 0.2819296736111110979, 3.821611111186975940, 0.1167790944451422425 ) ) ;
#18339 = ORIENTED_EDGE ( 'NONE', *, *, #4227, .F. ) ;
#18340 = CIRCLE ( 'NONE', #19891, 0.2500000000000000555 ) ;
#18341 = ORIENTED_EDGE ( 'NONE', *, *, #9519, .F. ) ;
#18342 = DATE_AND_TIME ( #20053, #9161 ) ;
#18343 = CARTESIAN_POINT ( 'NONE',  ( 0.4645997322662998585, -0.2720228281466835485, 0.05892894635879270676 ) ) ;
#18344 = CARTESIAN_POINT ( 'NONE',  ( -0.2722860045487212055, 4.951277928273133178, 0.1577204527339934603 ) ) ;
#18345 = DIRECTION ( 'NONE',  ( 0.000000000000000000, 0.000000000000000000, 1.000000000000000000 ) ) ;
#18346 = VERTEX_POINT ( 'NONE', #18256 ) ;
#18347 = CARTESIAN_POINT ( 'NONE',  ( -0.1292346314604056190, 0.1951388887371559855, -0.3119999999999999996 ) ) ;
#18348 = CARTESIAN_POINT ( 'NONE',  ( 0.3950000000000000178, 2.740039370078740433, -1.966000000000000192 ) ) ;
#18349 = CARTESIAN_POINT ( 'NONE',  ( -0.09970838333114330487, 5.126982898110991727, 0.2913680866046736151 ) ) ;
#18350 = CARTESIAN_POINT ( 'NONE',  ( -0.4687500000000003886, 0.2598076211353315679, 0.3779506566538943790 ) ) ;
#18351 = DIRECTION ( 'NONE',  ( 0.000000000000000000, 0.000000000000000000, -1.000000000000000000 ) ) ;
#18352 = PRODUCT_RELATED_PRODUCT_CATEGORY ( 'detail', '', ( #1355 ) ) ;
#18353 = VERTEX_POINT ( 'NONE', #20568 ) ;
#18354 = ORIENTED_EDGE ( 'NONE', *, *, #20764, .T. ) ;
#18355 = CARTESIAN_POINT ( 'NONE',  ( 0.2233192592356400275, 0.2366071427596004029, -0.3073725909049499494 ) ) ;
#18356 = CARTESIAN_POINT ( 'NONE',  ( 0.3091021031802769214, 5.086905331102652639, -0.04453840733622199677 ) ) ;
#18357 = CARTESIAN_POINT ( 'NONE',  ( 0.1144950937579609085, -0.2764156081756484751, 0.2168055555555584712 ) ) ;
#18358 = CARTESIAN_POINT ( 'NONE',  ( -0.2819296736111110424, 4.189666666742533074, 0.1167790944451424923 ) ) ;
#18359 = CARTESIAN_POINT ( 'NONE',  ( -0.2819296736111110979, 5.186194444520309865, 0.000000000000000000 ) ) ;
#18360 = CARTESIAN_POINT ( 'NONE',  ( 0.07165243469739802917, -0.2702856358549929894, 0.3907475393308576517 ) ) ;
#18361 = CARTESIAN_POINT ( 'NONE',  ( -0.2804485321785814000, 4.228482938243210754, 0.1413885024074663377 ) ) ;
#18362 = CARTESIAN_POINT ( 'NONE',  ( -1.910449006669871087E-17, 4.147999999999998799, -0.3119999999999999996 ) ) ;
#18363 = CARTESIAN_POINT ( 'NONE',  ( -0.3119999999999999996, 4.946611111262843252, 0.000000000000000000 ) ) ;
#18364 = CARTESIAN_POINT ( 'NONE',  ( 0.2819296736111110979, 5.061194444520310753, -3.452642723725051716E-17 ) ) ;
#18365 = EDGE_CURVE ( 'NONE', #9581, #8250, #1909, .T. ) ;
#18366 = CARTESIAN_POINT ( 'NONE',  ( 0.1292346314604007063, 4.866749999999998799, -0.3120000000000049400 ) ) ;
#18367 = ORIENTED_EDGE ( 'NONE', *, *, #23865, .F. ) ;
#18368 = DIRECTION ( 'NONE',  ( -0.000000000000000000, -1.000000000000000000, -0.000000000000000000 ) ) ;
#18369 = CARTESIAN_POINT ( 'NONE',  ( 0.1962369407262708754, 0.03892726110517438776, -0.2116860911888880925 ) ) ;
#18370 = ORIENTED_EDGE ( 'NONE', *, *, #4979, .T. ) ;
#18371 = CARTESIAN_POINT ( 'NONE',  ( 0.3155070326520292290, -0.1306872919485616569, 0.3678472222222264887 ) ) ;
#18372 = CARTESIAN_POINT ( 'NONE',  ( -0.1167790944451423535, 5.141055555631421470, 0.2819296736111110424 ) ) ;
#18373 = CARTESIAN_POINT ( 'NONE',  ( 0.1959149649064702292, -0.4281543196382478489, 0.4181366382341597521 ) ) ;
#18374 = EDGE_CURVE ( 'NONE', #10673, #2652, #1552, .T. ) ;
#18375 = LINE ( 'NONE', #1670, #903 ) ;
#18376 = CARTESIAN_POINT ( 'NONE',  ( 0.1167790944451423119, 0.1708333332574666907, -0.2819296736111110979 ) ) ;
#18377 = CARTESIAN_POINT ( 'NONE',  ( -0.1954553509668046918, -0.1954553509668046640, 0.1577777777777801815 ) ) ;
#18378 = CARTESIAN_POINT ( 'NONE',  ( 0.2819296736111110979, 5.172305555631421470, -3.452642723725051716E-17 ) ) ;
#18379 = DIRECTION ( 'NONE',  ( -0.000000000000000000, -1.000000000000000000, -0.000000000000000000 ) ) ;
#18380 = ORIENTED_EDGE ( 'NONE', *, *, #16946, .T. ) ;
#18381 = CARTESIAN_POINT ( 'NONE',  ( -0.1993543840281266355, 4.859805555631421470, 0.1993543840281267465 ) ) ;
#18382 = CARTESIAN_POINT ( 'NONE',  ( -0.3037999168084053458, 4.166440789197388028, -0.08196366530100891723 ) ) ;
#18383 = PLANE ( 'NONE',  #5854 ) ;
#18384 = CARTESIAN_POINT ( 'NONE',  ( 0.3119999999999999996, 4.578555555555555046, -3.820898013339742174E-17 ) ) ;
#18385 = CARTESIAN_POINT ( 'NONE',  ( 1.972470776266619596, 2.315961009048386643, -1.875610414248984004 ) ) ;
#18386 = CARTESIAN_POINT ( 'NONE',  ( 0.1292346314604056190, 4.644527777777776478, -0.3119999999999999996 ) ) ;
#18387 = CARTESIAN_POINT ( 'NONE',  ( 0.2819296736111110979, 3.991750000075865223, -3.452642723725051716E-17 ) ) ;
#18388 = CARTESIAN_POINT ( 'NONE',  ( -1.726321361862525858E-17, 3.852861111186976828, -0.2819296736111110979 ) ) ;
#18389 = CARTESIAN_POINT ( 'NONE',  ( 0.2274761419923447270, 4.036699467566920774, -0.2150353765082197166 ) ) ;
#18390 = CARTESIAN_POINT ( 'NONE',  ( -0.004206913933137605005, 0.5383631510497778327, 0.04698599556840143965 ) ) ;
#18391 = VERTEX_POINT ( 'NONE', #18617 ) ;
#18392 = CARTESIAN_POINT ( 'NONE',  ( 3.820898013339742174E-17, 5.384999999999999787, 0.3119999999999999996 ) ) ;
#18393 = ORIENTED_EDGE ( 'NONE', *, *, #16177, .T. ) ;
#18394 = CARTESIAN_POINT ( 'NONE',  ( -0.1167790944451423257, 4.342444444520310753, -0.2819296736111110424 ) ) ;
#18395 = CARTESIAN_POINT ( 'NONE',  ( 7.699581739047377146E-15, 4.099388889040679551, -0.3119999999999999996 ) ) ;
#18396 = ADVANCED_FACE ( 'NONE', ( #11065 ), #14855, .F. ) ;
#18397 = EDGE_CURVE ( 'NONE', #2181, #12390, #18739, .T. ) ;
#18398 = VECTOR ( 'NONE', #12433, 39.37007874015748143 ) ;
#18399 = LINE ( 'NONE', #100, #642 ) ;
#18400 = CARTESIAN_POINT ( 'NONE',  ( -0.1954553509668046640, 0.1954553509668046918, 0.2480555555555586933 ) ) ;
#18401 = CARTESIAN_POINT ( 'NONE',  ( -0.3119999857123673670, 3.945456803481290908, -0.04084082312690016925 ) ) ;
#18402 = EDGE_CURVE ( 'NONE', #14350, #9142, #18375, .T. ) ;
#18403 = CARTESIAN_POINT ( 'NONE',  ( -0.1917433973171703554, 4.438561529983626741, -0.2494925429433268727 ) ) ;
#18404 = CARTESIAN_POINT ( 'NONE',  ( 0.03651601414450977162, -0.2739930093161348501, 0.3880822748423153890 ) ) ;
#18405 = CARTESIAN_POINT ( 'NONE',  ( -0.2233192592356399997, 0.3437499999024575814, 0.3073725909049499494 ) ) ;
#18406 = CARTESIAN_POINT ( 'NONE',  ( 0.1993543840281266355, 0.2506944443685777957, 0.1993543840281267465 ) ) ;
#18407 = CARTESIAN_POINT ( 'NONE',  ( -0.2209708691207961095, 0.2209708691207961373, 0.1716666666666694097 ) ) ;
#18408 = DIRECTION ( 'NONE',  ( 0.000000000000000000, 1.000000000000000000, 0.000000000000000000 ) ) ;
#18409 = CARTESIAN_POINT ( 'NONE',  ( -0.06925083771014352296, 0.5795781470845841055, -0.7468261636789826907 ) ) ;
#18410 = CARTESIAN_POINT ( 'NONE',  ( 0.1144950937579609085, -0.2764156081756484751, -0.05402777777777704321 ) ) ;
#18411 = ORIENTED_EDGE ( 'NONE', *, *, #7472, .T. ) ;
#18412 = ORIENTED_EDGE ( 'NONE', *, *, #14678, .F. ) ;
#18413 = DIRECTION ( 'NONE',  ( 0.000000000000000000, -0.9961946980917454342, 0.08715574274765833240 ) ) ;
#18414 = CARTESIAN_POINT ( 'NONE',  ( -0.3119999999999998885, 4.720916666666666650, 0.1292346314604058410 ) ) ;
#18415 = CARTESIAN_POINT ( 'NONE',  ( -0.2819296736111110424, 0.5597222221463555858, -0.1167790944451423396 ) ) ;
#18416 = CARTESIAN_POINT ( 'NONE',  ( 0.1993543840281266633, 3.790361111186977272, -0.1993543840281266910 ) ) ;
#18417 = CARTESIAN_POINT ( 'NONE',  ( -0.2233192592356399442, 0.1794642856167432965, -0.3073725909049500049 ) ) ;
#18418 = AXIS2_PLACEMENT_3D ( 'NONE', #5246, #6969, #11110 ) ;
#18419 = CARTESIAN_POINT ( 'NONE',  ( -1.726321361862525858E-17, 4.352861111186976828, -0.2819296736111110979 ) ) ;
#18420 = DIRECTION ( 'NONE',  ( 0.000000000000000000, 0.000000000000000000, 1.000000000000000000 ) ) ;
#18421 = EDGE_CURVE ( 'NONE', #4536, #12538, #557, .T. ) ;
#18422 = DIRECTION ( 'NONE',  ( 0.4999999999999930611, 0.000000000000000000, 0.8660254037844425934 ) ) ;
#18423 = ORIENTED_EDGE ( 'NONE', *, *, #11416, .T. ) ;
#18424 = CARTESIAN_POINT ( 'NONE',  ( 0.2612248564553516506, 4.358128745886941324, 0.1706105875377467718 ) ) ;
#18425 = CARTESIAN_POINT ( 'NONE',  ( -0.1167790944451423535, 4.863277777853642903, 0.2819296736111110424 ) ) ;
#18426 = CARTESIAN_POINT ( 'NONE',  ( 0.001983654329502046367, 4.210443755940678656, -0.3119945956041611512 ) ) ;
#18427 = CARTESIAN_POINT ( 'NONE',  ( 0.3999999999999999667, 0.1821428571428570509, 0.1299678784931626307 ) ) ;
#18428 = CARTESIAN_POINT ( 'NONE',  ( -0.1167790944451423119, 4.564666666742532186, -0.2819296736111110979 ) ) ;
#18429 = APPROVAL_STATUS ( 'not_yet_approved' ) ;
#18430 = AXIS2_PLACEMENT_3D ( 'NONE', #6224, #13688, #21105 ) ;
#18431 = CARTESIAN_POINT ( 'NONE',  ( -0.4723836327791814949, 0.2801952116499777934, 0.04193567535760836518 ) ) ;
#18432 = CARTESIAN_POINT ( 'NONE',  ( -4.638126268221291196E-16, 0.06071428571428570675, -0.4000000000000000222 ) ) ;
#18433 = DIRECTION ( 'NONE',  ( 0.000000000000000000, 0.000000000000000000, 1.000000000000000000 ) ) ;
#18434 = EDGE_LOOP ( 'NONE', ( #21126, #2828 ) ) ;
#18435 = ORIENTED_EDGE ( 'NONE', *, *, #4886, .F. ) ;
#18436 = CARTESIAN_POINT ( 'NONE',  ( 0.1993543840281266355, 0.3201388888130222710, 0.1993543840281267465 ) ) ;
#18437 = LINE ( 'NONE', #7108, #14663 ) ;
#18438 = FACE_OUTER_BOUND ( 'NONE', #6970, .T. ) ;
#18439 = CARTESIAN_POINT ( 'NONE',  ( 0.1236067977499789861, 0.05714285714285712720, -0.3804226065180614236 ) ) ;
#18440 = CARTESIAN_POINT ( 'NONE',  ( 0.2977100099089716734, 3.700000000000000622, -0.09499999999999995948 ) ) ;
#18441 = CARTESIAN_POINT ( 'NONE',  ( -0.09537969278195178313, 3.879872140107286871, -0.2974432100491698483 ) ) ;
#18442 = CARTESIAN_POINT ( 'NONE',  ( 0.05000000000000028727, 0.000000000000000000, -2.194053356329904947 ) ) ;
#18443 = CARTESIAN_POINT ( 'NONE',  ( 0.2819296736111110979, 4.502166666742532186, 0.1167790944451422425 ) ) ;
#18444 = CARTESIAN_POINT ( 'NONE',  ( -0.3999999999999999667, 0.1374999998049151739, -0.1299678784931626030 ) ) ;
#18445 = DIRECTION ( 'NONE',  ( -0.000000000000000000, -0.000000000000000000, -1.000000000000000000 ) ) ;
#18446 = CARTESIAN_POINT ( 'NONE',  ( -0.1993543840281266355, 5.095916666742533074, 0.1993543840281267465 ) ) ;
#18447 = CARTESIAN_POINT ( 'NONE',  ( 0.1167790944451422702, 4.502166666742532186, -0.2819296736111110979 ) ) ;
#18448 = CARTESIAN_POINT ( 'NONE',  ( 0.1575217432702256393, 4.928054411463135054, -0.2724113156736405750 ) ) ;
#18449 = PERSON ( 'NAUO-PER7', 'UNSPECIFIED', 'UNSPECIFIED', ('UNSPECIFIED'), ('UNSPECIFIED'), ('UNSPECIFIED') ) ;
#18450 = CARTESIAN_POINT ( 'NONE',  ( -0.1292346314604058410, 0.4937499998482670627, 0.3119999999999998885 ) ) ;
#18451 = B_SPLINE_CURVE_WITH_KNOTS ( 'NONE', 3,
 ( #9375, #4002, #2186, #7895, #13535, #16929, #22293, #24114, #5588, #9496, #19004, #20829, #15346, #225, #17049, #18637, #7662, #9741, #343, #1807, #7428, #22773, #4241, #16818, #15112, #22538, #20472, #18517, #9252, #13292, #15229, #14990 ),
 .UNSPECIFIED., .F., .F.,
 ( 4, 2, 1, 1, 1, 1, 2, 2, 2, 2, 2, 2, 2, 2, 2, 2, 2, 4 ),
 ( 0.3746381435405087279, 0.3746563456430798134, 0.3746745477456508988, 0.3747109519507930697, 0.3747837603610774670, 0.3749293771816462062, 0.3752206108227836290, 0.3758030781050585301, 0.3769680126696083322, 0.3792978817987079920, 0.3816277509278076518, 0.3839576200569072562, 0.3845400873391821572, 0.3851225546214570583, 0.3862874891860069160, 0.3886173583151065203, 0.3909472274442061801, 0.3932770965733057844 ),
 .UNSPECIFIED. ) ;
#18452 = CARTESIAN_POINT ( 'NONE',  ( 0.06495106723445233377, 3.906766557144303764, 0.3070669447693011866 ) ) ;
#18453 = CARTESIAN_POINT ( 'NONE',  ( -0.2206173157302028232, 4.384111111262843252, -0.2206173157302028232 ) ) ;
#18454 = VECTOR ( 'NONE', #1107, 39.37007874015748143 ) ;
#18455 = CARTESIAN_POINT ( 'NONE',  ( 0.1167790944451422702, 4.460500000075867000, -0.2819296736111110979 ) ) ;
#18456 = CARTESIAN_POINT ( 'NONE',  ( 0.2819296736111110979, 3.936194444520309865, -3.452642723725051716E-17 ) ) ;
#18457 = EDGE_LOOP ( 'NONE', ( #8559, #5299, #2982, #6498 ) ) ;
#18458 = ORIENTED_EDGE ( 'NONE', *, *, #9010, .F. ) ;
#18459 = VERTEX_POINT ( 'NONE', #6288 ) ;
#18460 = EDGE_CURVE ( 'NONE', #22975, #3340, #5713, .T. ) ;
#18461 = PERSON_AND_ORGANIZATION ( #15518, #2538 ) ;
#18462 = CARTESIAN_POINT ( 'NONE',  ( 0.000000000000000000, 5.384999999999999787, 0.000000000000000000 ) ) ;
#18463 = EDGE_CURVE ( 'NONE', #9585, #18353, #443, .T. ) ;
#18464 = CARTESIAN_POINT ( 'NONE',  ( 0.1292346314604058410, 4.234805555555554157, 0.3119999999999998885 ) ) ;
#18465 = DIRECTION ( 'NONE',  ( -1.000000000000000000, 0.000000000000000000, -0.000000000000000000 ) ) ;
#18466 = ORIENTED_EDGE ( 'NONE', *, *, #14666, .F. ) ;
#18467 = CARTESIAN_POINT ( 'NONE',  ( 0.3119999999999999996, 0.5111111109593782231, 0.000000000000000000 ) ) ;
#18468 = CARTESIAN_POINT ( 'NONE',  ( 0.000000000000000000, 0.9099999999999988098, 0.000000000000000000 ) ) ;
#18469 = CARTESIAN_POINT ( 'NONE',  ( -0.2962237115742567539, 3.727440431103998808, 0.1082426406064014301 ) ) ;
#18470 = VECTOR ( 'NONE', #13939, 39.37007874015748143 ) ;
#18471 = LINE ( 'NONE', #9447, #22537 ) ;
#18472 = ORIENTED_EDGE ( 'NONE', *, *, #3343, .F. ) ;
#18473 = CARTESIAN_POINT ( 'NONE',  ( -0.2923287055106771337, 0.1258928570453147489, 0.2123892367102619971 ) ) ;
#18474 = CARTESIAN_POINT ( 'NONE',  ( 0.1816571697360684357, 5.094271231115367726, -0.2535119103260691786 ) ) ;
#18475 = CARTESIAN_POINT ( 'NONE',  ( 0.1954553509668047195, 0.1954553509668046085, 0.2897222222222257115 ) ) ;
#18476 = B_SPLINE_CURVE_WITH_KNOTS ( 'NONE', 3,
 ( #19736, #11838, #21209, #2790, #12085, #10128, #15487, #3365, #21088, #4378, #10244, #10009, #19615, #8388, #2908, #725, #10366, #6689, #21564, #17432, #9222, #24083, #5677, #7154, #2022, #11295, #1777, #14956, #7274, #9341, #20318, #16424, #18483, #14843, #11178, #64, #185, #15076, #9092 ),
 .UNSPECIFIED., .F., .F.,
 ( 4, 2, 2, 2, 2, 2, 1, 1, 1, 1, 2, 2, 1, 2, 2, 2, 2, 2, 2, 2, 2, 4 ),
 ( 0.2649879068747749700, 0.2673297384506001517, 0.2696715700264253890, 0.2720134016022505707, 0.2731843173901631894, 0.2743552331780757525, 0.2745015976515648437, 0.2745747798883093616, 0.2746113710066816482, 0.2746205187862747477, 0.2746250926760712696, 0.2746296665658677916, 0.2746479621250539349, 0.2749406910720321173, 0.2755261489659885932, 0.2766970647539014894, 0.2778679805418143300, 0.2790388963297272262, 0.2802098121176401224, 0.2813807279055530186, 0.2825516436934658593, 0.2837225594813787555 ),
 .UNSPECIFIED. ) ;
#18477 = CARTESIAN_POINT ( 'NONE',  ( 0.2819296736111110424, 4.273000000075865223, -0.1167790944451423396 ) ) ;
#18478 = CARTESIAN_POINT ( 'NONE',  ( 0.1993543840281266633, 5.054250000075865223, -0.1993543840281266910 ) ) ;
#18479 = CARTESIAN_POINT ( 'NONE',  ( 0.03651601414450977162, -0.2739930093161348501, 0.3880822748423153890 ) ) ;
#18480 = CARTESIAN_POINT ( 'NONE',  ( -0.3120253914852480492, 4.224625367392181197, 0.009383917684771203582 ) ) ;
#18481 = CARTESIAN_POINT ( 'NONE',  ( -1.910449006669871087E-17, 3.814666666666665762, -0.3119999999999999996 ) ) ;
#18482 = CARTESIAN_POINT ( 'NONE',  ( -0.3119999999999999996, 4.891055555707287894, 0.000000000000000000 ) ) ;
#18483 = CARTESIAN_POINT ( 'NONE',  ( 0.2252594654730211976, 4.800977599731078627, 0.2171865793878193507 ) ) ;
#18484 = DIRECTION ( 'NONE',  ( -0.000000000000000000, -1.000000000000000000, -0.000000000000000000 ) ) ;
#18485 = EDGE_LOOP ( 'NONE', ( #18222, #12536, #3337, #20912 ) ) ;
#18486 = DIRECTION ( 'NONE',  ( 0.000000000000000000, 0.000000000000000000, -1.000000000000000000 ) ) ;
#18487 = CIRCLE ( 'NONE', #8741, 1.223000000000000309 ) ;
#18488 = CC_DESIGN_PERSON_AND_ORGANIZATION_ASSIGNMENT ( #7722, #11271, ( #2989 ) ) ;
#18489 = CARTESIAN_POINT ( 'NONE',  ( 0.2839242323463955775, 0.03423162783098992329, 0.004826162406255454784 ) ) ;
#18490 = ORIENTED_EDGE ( 'NONE', *, *, #20927, .F. ) ;
#18491 = CARTESIAN_POINT ( 'NONE',  ( -0.2230971623002954152, -0.2230971623002953874, 0.2949305555555592484 ) ) ;
#18492 = CARTESIAN_POINT ( 'NONE',  ( -0.2819296736111110979, 5.019527777853642903, 0.000000000000000000 ) ) ;
#18493 = VERTEX_POINT ( 'NONE', #7761 ) ;
#18494 = CARTESIAN_POINT ( 'NONE',  ( -0.3613381517857143232, 0.3866071427596004528, -4.425116109941954795E-17 ) ) ;
#18495 = EDGE_LOOP ( 'NONE', ( #23848, #9948, #12297, #11627, #2115 ) ) ;
#18496 = CARTESIAN_POINT ( 'NONE',  ( 0.1167790944451423119, 0.3374999999241333759, -0.2819296736111110979 ) ) ;
#18497 = CARTESIAN_POINT ( 'NONE',  ( 0.2764156081756483641, 0.1144950937579610056, 0.1820833333333359283 ) ) ;
#18498 = CARTESIAN_POINT ( 'NONE',  ( 0.1993543840281266633, 4.957027777853642903, -0.1993543840281266910 ) ) ;
#18499 = CARTESIAN_POINT ( 'NONE',  ( 0.5997114317030027841, 0.000000000000000000, -0.9454293994002404000 ) ) ;
#18500 = AXIS2_PLACEMENT_3D ( 'NONE', #2889, #6548, #10347 ) ;
#18501 = ORIENTED_EDGE ( 'NONE', *, *, #4976, .F. ) ;
#18502 = CARTESIAN_POINT ( 'NONE',  ( -0.1167790944451423535, 4.863277777853642903, 0.2819296736111110424 ) ) ;
#18503 = CARTESIAN_POINT ( 'NONE',  ( -0.3999999999999999667, 0.06607142837634374932, -0.1299678784931626030 ) ) ;
#18504 = DIRECTION ( 'NONE',  ( 0.5000000000000037748, 0.000000000000000000, 0.8660254037844362651 ) ) ;
#18505 = DIRECTION ( 'NONE',  ( 0.000000000000000000, 0.000000000000000000, 1.000000000000000000 ) ) ;
#18506 = CARTESIAN_POINT ( 'NONE',  ( -5.731347020009612645E-17, 0.5527777776260448528, 0.3119999999999999996 ) ) ;
#18507 = CARTESIAN_POINT ( 'NONE',  ( 0.3119999999999999996, 4.467444444444443441, -3.820898013339742174E-17 ) ) ;
#18508 = CARTESIAN_POINT ( 'NONE',  ( 0.1167790944451424506, 3.981333333409199593, 0.2819296736111110424 ) ) ;
#18509 = CARTESIAN_POINT ( 'NONE',  ( -0.2819296736111110424, 3.814666666742532630, 0.1167790944451424923 ) ) ;
#18510 = CARTESIAN_POINT ( 'NONE',  ( 0.08174725030332795350, 4.018423240896470183, 0.3038629659492873003 ) ) ;
#18511 = CYLINDRICAL_SURFACE ( 'NONE', #22998, 0.3119999999999999996 ) ;
#18512 = LOCAL_TIME ( 21, 9, 13.00000000000000000, #22976 ) ;
#18513 = DIRECTION ( 'NONE',  ( 0.000000000000000000, 0.000000000000000000, 1.000000000000000000 ) ) ;
#18514 = ADVANCED_FACE ( 'NONE', ( #13512 ), #13976, .F. ) ;
#18515 = DIRECTION ( 'NONE',  ( -1.000000000000000000, 0.000000000000000000, 6.148297094540788948E-16 ) ) ;
#18516 = AXIS2_PLACEMENT_3D ( 'NONE', #2132, #18960, #17005 ) ;
#18517 = CARTESIAN_POINT ( 'NONE',  ( 0.2022309808788627650, 4.633432797117196245, 0.2408951298654545825 ) ) ;
#18518 = CARTESIAN_POINT ( 'NONE',  ( 0.2764156081756483641, -0.1144950937579611167, 0.1681944444444469777 ) ) ;
#18519 = CARTESIAN_POINT ( 'NONE',  ( 0.6107956263425956545, 2.685901063997346405, -1.186814756611144883 ) ) ;
#18520 = CARTESIAN_POINT ( 'NONE',  ( -0.1571332995722349857, 4.437395902338867160, -0.2726191217874048278 ) ) ;
#18521 = SHAPE_REPRESENTATION ( 'MAS-409-Body', ( #9127 ), #558 ) ;
#18522 = CARTESIAN_POINT ( 'NONE',  ( 0.000000000000000000, 0.2764156081756484196, 0.3591666666666706309 ) ) ;
#18523 = APPROVAL_PERSON_ORGANIZATION ( #19900, #5231, #21963 ) ;
#18524 = CARTESIAN_POINT ( 'NONE',  ( -0.2233192592356399997, 0.2008928570453147322, 0.3073725909049499494 ) ) ;
#18525 = CARTESIAN_POINT ( 'NONE',  ( 0.2819296736111110979, 0.3131944443685777957, 0.000000000000000000 ) ) ;
#18526 = CARTESIAN_POINT ( 'NONE',  ( -0.3125000000000000000, 1.913510623667739771E-17, 0.1786111111111139127 ) ) ;
#18527 = DIRECTION ( 'NONE',  ( 0.000000000000000000, 0.000000000000000000, 1.000000000000000000 ) ) ;
#18528 = CARTESIAN_POINT ( 'NONE',  ( 0.04615996209784178905, 0.5146154108223025547, 0.3902123106865083013 ) ) ;
#18529 = CARTESIAN_POINT ( 'NONE',  ( -0.1954553509668046640, 0.1954553509668046918, -0.02277777777777679341 ) ) ;
#18530 = VERTEX_POINT ( 'NONE', #11920 ) ;
#18531 = ORIENTED_EDGE ( 'NONE', *, *, #5743, .T. ) ;
#18532 = DIRECTION ( 'NONE',  ( 1.000000000000000000, -0.000000000000000000, 1.224646799147353207E-16 ) ) ;
#18533 = FACE_OUTER_BOUND ( 'NONE', #563, .T. ) ;
#18534 = CARTESIAN_POINT ( 'NONE',  ( -0.1292346314604056190, 0.03541666666666633267, -0.3119999999999999996 ) ) ;
#18535 = CARTESIAN_POINT ( 'NONE',  ( -0.2819296736111110424, 3.870222222298087988, 0.1167790944451424923 ) ) ;
#18536 = CARTESIAN_POINT ( 'NONE',  ( 0.1116596296178199027, 0.1401785713310290393, 0.3436530038418508792 ) ) ;
#18537 = VERTEX_POINT ( 'NONE', #15324 ) ;
#18538 = CARTESIAN_POINT ( 'NONE',  ( 0.1167790944451422702, 4.516055555631421470, -0.2819296736111110424 ) ) ;
#18539 = FACE_OUTER_BOUND ( 'NONE', #6451, .T. ) ;
#18540 = DIRECTION ( 'NONE',  ( -0.8651979924482653406, 0.04370253788966859537, 0.4995222938423205528 ) ) ;
#18541 = ORIENTED_EDGE ( 'NONE', *, *, #16115, .F. ) ;
#18542 = LINE ( 'NONE', #1832, #2713 ) ;
#18543 = CARTESIAN_POINT ( 'NONE',  ( -0.2819296736111110424, 4.849388888964755395, -0.1167790944451423119 ) ) ;
#18544 = EDGE_CURVE ( 'NONE', #11560, #14570, #23681, .T. ) ;
#18545 = CARTESIAN_POINT ( 'NONE',  ( -0.3008913205206853458, 5.155183786276188229, -0.01229715577229057756 ) ) ;
#18546 = DIRECTION ( 'NONE',  ( 0.000000000000000000, 0.000000000000000000, 1.000000000000000000 ) ) ;
#18547 = CARTESIAN_POINT ( 'NONE',  ( 0.3236067977499789694, 0.2410714283763437382, 0.2351141009169893659 ) ) ;
#18548 = LINE ( 'NONE', #13203, #23904 ) ;
#18549 = CIRCLE ( 'NONE', #23202, 0.3125000000000000000 ) ;
#18550 = CARTESIAN_POINT ( 'NONE',  ( -0.1167790944451423535, 4.752166666742531298, 0.2819296736111110979 ) ) ;
#18551 = DIRECTION ( 'NONE',  ( 1.000000000000000000, 0.000000000000000000, 0.000000000000000000 ) ) ;
#18552 = CARTESIAN_POINT ( 'NONE',  ( 0.1292346314604000956, 4.922305555555555046, -0.3120000000000054952 ) ) ;
#18553 = CARTESIAN_POINT ( 'NONE',  ( 1.726321361862525858E-17, 0.5076388888130222155, -0.2819296736111110979 ) ) ;
#18554 = EDGE_LOOP ( 'NONE', ( #12109, #3908, #11066 ) ) ;
#18555 = ORIENTED_EDGE ( 'NONE', *, *, #16478, .T. ) ;
#18556 = CARTESIAN_POINT ( 'NONE',  ( 0.1993543840281266910, 0.2784722221463555858, -0.1993543840281266910 ) ) ;
#18557 = CARTESIAN_POINT ( 'NONE',  ( 2.285240235267019138, 2.686579321989253089, -2.477179094559016193 ) ) ;
#18558 = CARTESIAN_POINT ( 'NONE',  ( -0.02753534767366182245, 5.190979356084988616, -0.2888344835192422910 ) ) ;
#18559 = CARTESIAN_POINT ( 'NONE',  ( 0.3999999999999999667, 0.1107142857142856956, 0.1299678784931626307 ) ) ;
#18560 = CARTESIAN_POINT ( 'NONE',  ( 0.2230971623002953874, -0.2230971623002954429, -0.08354166666666636154 ) ) ;
#18561 = CARTESIAN_POINT ( 'NONE',  ( -0.4593750000000005329, -0.2760455974562900372, 0.06112444011295364160 ) ) ;
#18562 = EDGE_CURVE ( 'NONE', #20999, #16665, #18982, .T. ) ;
#18563 = DIRECTION ( 'NONE',  ( -0.5000000000000003331, 0.000000000000000000, -0.8660254037844384856 ) ) ;
#18564 = CARTESIAN_POINT ( 'NONE',  ( 0.1167790944451423535, 0.3027777777019111105, 0.2819296736111110979 ) ) ;
#18565 = CARTESIAN_POINT ( 'NONE',  ( -0.2819296736111110979, 0.01111111103524447911, 0.1167790944451422425 ) ) ;
#18566 = ADVANCED_FACE ( 'NONE', ( #19340 ), #17506, .F. ) ;
#18567 = CARTESIAN_POINT ( 'NONE',  ( -1.726321361862525858E-17, 4.519527777853643791, -0.2819296736111110979 ) ) ;
#18568 = CARTESIAN_POINT ( 'NONE',  ( 0.3236067977499789694, 0.02678571409062949910, 0.2351141009169893659 ) ) ;
#18569 = CARTESIAN_POINT ( 'NONE',  ( 0.000000000000000000, 0.000000000000000000, 0.2041999999999999926 ) ) ;
#18570 = CARTESIAN_POINT ( 'NONE',  ( -1.726321361862525858E-17, 5.019527777853643791, -0.2819296736111110979 ) ) ;
#18571 = CARTESIAN_POINT ( 'NONE',  ( -0.2819296736111110979, 4.404944444520309865, -0.1167790944451422980 ) ) ;
#18572 = CARTESIAN_POINT ( 'NONE',  ( 0.08942137597415596162, 3.740864561460785165, 0.2997242127448243032 ) ) ;
#18573 = DIRECTION ( 'NONE',  ( -0.000000000000000000, -0.000000000000000000, 1.000000000000000000 ) ) ;
#18574 = CIRCLE ( 'NONE', #13913, 1.243000000000000105 ) ;
#18575 = CARTESIAN_POINT ( 'NONE',  ( 0.02489560895761679105, 3.932016240302184773, -0.3119999658293151068 ) ) ;
#18576 = CARTESIAN_POINT ( 'NONE',  ( -0.3119999999999999996, 4.002166666818398610, 0.000000000000000000 ) ) ;
#18577 = EDGE_CURVE ( 'NONE', #1519, #16287, #12146, .T. ) ;
#18578 = CARTESIAN_POINT ( 'NONE',  ( -0.1167790944451423535, 4.599388888964754507, 0.2819296736111110979 ) ) ;
#18579 = CARTESIAN_POINT ( 'NONE',  ( -0.1236067977499790416, 0.2982142855192009279, 0.3804226065180614236 ) ) ;
#18580 = ORIENTED_EDGE ( 'NONE', *, *, #8731, .T. ) ;
#18581 = ORIENTED_EDGE ( 'NONE', *, *, #5929, .F. ) ;
#18582 = VERTEX_POINT ( 'NONE', #21744 ) ;
#18583 = COORDINATED_UNIVERSAL_TIME_OFFSET ( 0, 0, .AHEAD. ) ;
#18584 = CARTESIAN_POINT ( 'NONE',  ( 5.731347020009612645E-17, 4.286888888888888083, 0.3119999999999999996 ) ) ;
#18585 = CARTESIAN_POINT ( 'NONE',  ( -0.09230038814513606693, 4.846752338702703611, 0.2982970817797798713 ) ) ;
#18586 = CARTESIAN_POINT ( 'NONE',  ( 0.000000000000000000, 0.06786299768266475241, 0.000000000000000000 ) ) ;
#18587 = ORIENTED_EDGE ( 'NONE', *, *, #22918, .F. ) ;
#18588 = CARTESIAN_POINT ( 'NONE',  ( 0.3119999999999999996, 0.4555555554038225874, 0.000000000000000000 ) ) ;
#18589 = CIRCLE ( 'NONE', #13540, 0.2499999999999999722 ) ;
#18590 = EDGE_LOOP ( 'NONE', ( #14051, #2113, #21122, #9613 ) ) ;
#18591 = DIRECTION ( 'NONE',  ( -0.000000000000000000, -1.000000000000000000, -0.000000000000000000 ) ) ;
#18592 = CARTESIAN_POINT ( 'NONE',  ( 0.5129115487115525340, 2.693521551442877193, -0.7037288651031901043 ) ) ;
#18593 = CARTESIAN_POINT ( 'NONE',  ( 0.3125000000000002220, -0.1294417382415921358, -0.08180555555555521496 ) ) ;
#18594 = CARTESIAN_POINT ( 'NONE',  ( 0.2496703805607334292, 3.980133472758900393, -0.1915199933392999210 ) ) ;
#18595 = ORIENTED_EDGE ( 'NONE', *, *, #19502, .T. ) ;
#18596 = CARTESIAN_POINT ( 'NONE',  ( 0.3613381517857143232, 0.08303571418817189131, 0.000000000000000000 ) ) ;
#18597 = VERTEX_POINT ( 'NONE', #16500 ) ;
#18598 = CARTESIAN_POINT ( 'NONE',  ( 0.03852881856483229839, 5.098954151918542621, -0.3091372944403406042 ) ) ;
#18599 = CARTESIAN_POINT ( 'NONE',  ( 0.1954553509668047195, 0.1954553509668046085, 0.1786111111111137462 ) ) ;
#18600 = CARTESIAN_POINT ( 'NONE',  ( -1.726321361862525858E-17, 4.283416666742532186, -0.2819296736111110979 ) ) ;
#18601 = CARTESIAN_POINT ( 'NONE',  ( 0.1993543840281266633, 5.109805555631420582, -0.1993543840281266910 ) ) ;
#18602 = DIRECTION ( 'NONE',  ( 0.000000000000000000, -0.000000000000000000, -1.000000000000000000 ) ) ;
#18603 = CARTESIAN_POINT ( 'NONE',  ( 0.3119999999999999996, 3.804249999999999243, -0.1292346314604056745 ) ) ;
#18604 = EDGE_CURVE ( 'NONE', #1635, #19685, #23864, .T. ) ;
#18605 = CARTESIAN_POINT ( 'NONE',  ( -0.3119999999999999996, 4.720916666818398610, -0.1292346314604056468 ) ) ;
#18606 = CARTESIAN_POINT ( 'NONE',  ( -0.2819296736111110979, 5.141055555631421470, -0.1167790944451422980 ) ) ;
#18607 = VECTOR ( 'NONE', #22495, 39.37007874015748143 ) ;
#18608 = DIRECTION ( 'NONE',  ( 0.000000000000000000, 0.000000000000000000, 1.000000000000000000 ) ) ;
#18609 = ORIENTED_EDGE ( 'NONE', *, *, #22139, .F. ) ;
#18610 = CARTESIAN_POINT ( 'NONE',  ( -0.1116596296178200276, 0.1866071427596004417, 0.3436530038418508792 ) ) ;
#18611 = CARTESIAN_POINT ( 'NONE',  ( 2.295391506243690927, 2.740000000000000213, -2.409633369868423358 ) ) ;
#18612 = ORIENTED_EDGE ( 'NONE', *, *, #13651, .T. ) ;
#18613 = PERSON_AND_ORGANIZATION_ROLE ( 'design_supplier' ) ;
#18614 = CARTESIAN_POINT ( 'NONE',  ( 0.000000000000000000, 0.3155070326520292845, 0.2185416666666697982 ) ) ;
#18615 = CARTESIAN_POINT ( 'NONE',  ( -0.1167790944451423257, 5.175777777853644679, -0.2819296736111110424 ) ) ;
#18616 = CARTESIAN_POINT ( 'NONE',  ( 2.386814157129576675, 0.000000000000000000, -2.935999999999999943 ) ) ;
#18617 = CARTESIAN_POINT ( 'NONE',  ( -0.009374999999999907713, -0.5358532185916218271, 0.3779506566538943235 ) ) ;
#18618 = AXIS2_PLACEMENT_3D ( 'NONE', #13288, #575, #3994 ) ;
#18619 = CARTESIAN_POINT ( 'NONE',  ( 0.1167790944451423535, 0.3166666665908000056, 0.2819296736111110979 ) ) ;
#18620 = CARTESIAN_POINT ( 'NONE',  ( -0.1954553509668046918, -0.1954553509668046640, 0.3244444444444481435 ) ) ;
#18621 = CARTESIAN_POINT ( 'NONE',  ( -0.1993543840281266910, 4.970916666742532186, -0.1993543840281266910 ) ) ;
#18622 = LINE ( 'NONE', #18261, #18655 ) ;
#18623 = CARTESIAN_POINT ( 'NONE',  ( -0.2819296736111110979, 4.852861111186976828, 0.000000000000000000 ) ) ;
#18624 = CYLINDRICAL_SURFACE ( 'NONE', #23127, 0.3119999999999999996 ) ;
#18625 =( BOUNDED_SURFACE ( )  B_SPLINE_SURFACE ( 1, 2, ( 
 ( #22218, #20278, #14554, #5272, #7351, #3564, #5518, #12981, #3689, #18565, #14682, #20398, #22336, #11018, #20, #5639, #18683, #20517, #9056, #22099, #11136, #7588, #1984, #1854, #3933, #16503, #11376, #15039, #16860, #22462, #12742, #13221, #3445, #20632, #8937, #10896, #23914, #7235, #5395, #17101, #17222, #13580, #22937, #6111, #6233, #20990, #13698, #506, #269, #19049, #11992, #13456, #21115, #22821, #17457, #9791, #388, #20873, #7827, #13332, #4405, #9907, #2099, #2589, #9540, #8178, #8063, #15393, #5870, #16973, #11741, #11868, #4167, #18933, #19282, #6358, #19163, #7939, #10035, #11617, #2351, #5991, #2470, #15511, #4286, #17339, #750, #632, #15632, #21239, #2231, #4529, #23050, #13805, #7708, #15155, #22585, #20754, #4045, #11498, #9663, #15273, #22701, #3061, #10272, #10397, #6715, #16109, #23407, #23522, #14160, #6839, #17820, #17578, #12230, #5118, #6596, #14279, #15986, #10626, #2939, #17697, #14044, #989, #6475, #21717, #10508, #19404, #19883, #2703, #1351, #1235, #8544, #23165, #10154, #4883, #5000, #21475, #12113, #12462, #23644, #12348, #1110, #3176, #4758, #19640, #23282, #19765, #8660, #21590, #17939, #2816, #18055, #8782, #16234, #14404, #6963, #13928, #868, #21358, #21828, #8301, #15753, #4646, #19523, #8418, #15866, #18415, #3781, #12954, #20007, #1472, #12830, #20366, #22430, #5365, #7323, #7441, #12712, #16473, #1709 ),
 ( #9148, #7557, #18653, #10990, #7202, #18297, #16591, #23883, #10747, #3293, #22069, #14648, #24013, #14774, #22189, #5488, #1595, #3657, #1824, #20249, #11104, #18534, #14888, #24126, #5240, #9030, #9269, #16709, #3418, #3537, #22307, #5605, #13070, #20485, #11225, #1946, #9392, #18179, #16832, #12584, #115, #15010, #8909, #16353, #23764, #10868, #7085, #14524, #21947, #20126, #13550, #15600, #6203, #13190, #11831, #11709, #19022, #9510, #20604, #15361, #600, #17064, #22553, #8031, #10003, #22790, #20844, #2436, #357, #7798, #9634, #6083, #19132, #4134, #15241, #13307, #20964, #4258, #19250, #720, #11591, #16943, #3901, #242, #2317, #13669, #15482, #2556, #22671, #9878, #15127, #9754, #21083, #17307, #11346, #18773, #5960, #22908, #5731, #13422, #477, #4373, #5844, #17191, #7909, #17427, #2069, #7677, #8148, #20722, #4018, #11468, #18901, #2201, #21442, #17665, #4615, #12200, #10237, #21203, #6324, #8382, #951, #4728, #19607, #17784, #8508, #12077, #10361, #12316, #15832, #6683, #4848, #17908, #10478, #15718, #19490, #23251, #14249, #21557, #1077, #18024, #23132, #1321, #21684, #16079, #14011, #13776, #19848, #17547, #6561, #10596, #1203, #2672, #8634, #10122, #15949, #14128, #13897, #2902, #23375, #19728, #3031, #23491, #6807, #4967, #12434, #4495, #3146, #8746, #23023, #11960, #19375, #840, #8269, #21326, #6445, #2784, #3262, #3626, #23985 ) ),
 .UNSPECIFIED., .F., .F., .F. ) 
 B_SPLINE_SURFACE_WITH_KNOTS ( ( 2, 2 ),
 ( 3, 2, 2, 2, 2, 2, 2, 2, 2, 2, 2, 2, 2, 2, 2, 2, 2, 2, 2, 2, 2, 2, 2, 2, 2, 2, 2, 2, 2, 2, 2, 2, 2, 2, 2, 2, 2, 2, 2, 2, 2, 2, 2, 2, 2, 2, 2, 2, 2, 2, 2, 2, 2, 2, 2, 2, 2, 2, 2, 2, 2, 2, 2, 2, 2, 2, 2, 2, 2, 2, 2, 2, 2, 2, 2, 2, 2, 2, 2, 2, 2, 2, 2, 2, 2, 2, 2, 2, 2, 2, 3 ),
 ( 0.000000000000000000, 1.000000000000000000 ),
 ( 0.000000000000000000, 0.01041666666666666609, 0.02083333333333333218, 0.03125000000000000000, 0.04166666666666666435, 0.05208333333333333565, 0.06250000000000000000, 0.07291666666666667129, 0.08333333333333332871, 0.09375000000000000000, 0.1041666666666666713, 0.1145833333333333287, 0.1250000000000000000, 0.1354166666666666574, 0.1458333333333333426, 0.1562500000000000000, 0.1666666666666666574, 0.1770833333333333426, 0.1875000000000000000, 0.1979166666666666574, 0.2083333333333333426, 0.2187500000000000000, 0.2291666666666666574, 0.2395833333333333426, 0.2500000000000000000, 0.2604166666666666852, 0.2708333333333333148, 0.2812500000000000000, 0.2916666666666666852, 0.3020833333333333148, 0.3125000000000000000, 0.3229166666666666852, 0.3333333333333333148, 0.3437500000000000000, 0.3541666666666666852, 0.3645833333333333148, 0.3750000000000000000, 0.3854166666666666852, 0.3958333333333333148, 0.4062500000000000000, 0.4166666666666666852, 0.4270833333333333148, 0.4375000000000000000, 0.4479166666666666852, 0.4583333333333333148, 0.4687500000000000000, 0.4791666666666666852, 0.4895833333333333148, 0.5000000000000000000, 0.5104166666666666297, 0.5208333333333333703, 0.5312500000000000000, 0.5416666666666666297, 0.5520833333333333703, 0.5625000000000000000, 0.5729166666666666297, 0.5833333333333333703, 0.5937500000000000000, 0.6041666666666666297, 0.6145833333333333703, 0.6250000000000000000, 0.6354166666666666297, 0.6458333333333333703, 0.6562500000000000000, 0.6666666666666666297, 0.6770833333333333703, 0.6875000000000000000, 0.6979166666666666297, 0.7083333333333333703, 0.7187500000000000000, 0.7291666666666666297, 0.7395833333333333703, 0.7500000000000000000, 0.7604166666666666297, 0.7708333333333333703, 0.7812500000000000000, 0.7916666666666666297, 0.8020833333333333703, 0.8125000000000000000, 0.8229166666666666297, 0.8333333333333333703, 0.8437500000000000000, 0.8541666666666666297, 0.8645833333333333703, 0.8750000000000000000, 0.8854166666666666297, 0.8958333333333333703, 0.9062500000000000000, 0.9166666666666666297, 0.9270833333333333703, 0.9375000000000000000 ),
 .UNSPECIFIED. ) 
 GEOMETRIC_REPRESENTATION_ITEM ( )  RATIONAL_B_SPLINE_SURFACE ( (
 ( 1.000000000000000000, 0.9238795325112867385, 1.000000000000000000, 0.9238795325112867385, 1.000000000000000000, 0.9238795325112867385, 1.000000000000000000, 0.9238795325112867385, 1.000000000000000000, 0.9238795325112867385, 1.000000000000000000, 0.9238795325112867385, 1.000000000000000000, 0.9238795325112867385, 1.000000000000000000, 0.9238795325112867385, 1.000000000000000000, 0.9238795325112867385, 1.000000000000000000, 0.9238795325112867385, 1.000000000000000000, 0.9238795325112867385, 1.000000000000000000, 0.9238795325112867385, 1.000000000000000000, 0.9238795325112867385, 1.000000000000000000, 0.9238795325112867385, 1.000000000000000000, 0.9238795325112867385, 1.000000000000000000, 0.9238795325112867385, 1.000000000000000000, 0.9238795325112867385, 1.000000000000000000, 0.9238795325112867385, 1.000000000000000000, 0.9238795325112867385, 1.000000000000000000, 0.9238795325112867385, 1.000000000000000000, 0.9238795325112867385, 1.000000000000000000, 0.9238795325112867385, 1.000000000000000000, 0.9238795325112867385, 1.000000000000000000, 0.9238795325112867385, 1.000000000000000000, 0.9238795325112867385, 1.000000000000000000, 0.9238795325112867385, 1.000000000000000000, 0.9238795325112867385, 1.000000000000000000, 0.9238795325112867385, 1.000000000000000000, 0.9238795325112867385, 1.000000000000000000, 0.9238795325112867385, 1.000000000000000000, 0.9238795325112867385, 1.000000000000000000, 0.9238795325112867385, 1.000000000000000000, 0.9238795325112867385, 1.000000000000000000, 0.9238795325112867385, 1.000000000000000000, 0.9238795325112867385, 1.000000000000000000, 0.9238795325112867385, 1.000000000000000000, 0.9238795325112867385, 1.000000000000000000, 0.9238795325112867385, 1.000000000000000000, 0.9238795325112867385, 1.000000000000000000, 0.9238795325112867385, 1.000000000000000000, 0.9238795325112867385, 1.000000000000000000, 0.9238795325112867385, 1.000000000000000000, 0.9238795325112867385, 1.000000000000000000, 0.9238795325112867385, 1.000000000000000000, 0.9238795325112867385, 1.000000000000000000, 0.9238795325112867385, 1.000000000000000000, 0.9238795325112867385, 1.000000000000000000, 0.9238795325112867385, 1.000000000000000000, 0.9238795325112867385, 1.000000000000000000, 0.9238795325112867385, 1.000000000000000000, 0.9238795325112867385, 1.000000000000000000, 0.9238795325112867385, 1.000000000000000000, 0.9238795325112867385, 1.000000000000000000, 0.9238795325112867385, 1.000000000000000000, 0.9238795325112867385, 1.000000000000000000, 0.9238795325112867385, 1.000000000000000000, 0.9238795325112867385, 1.000000000000000000, 0.9238795325112867385, 1.000000000000000000, 0.9238795325112867385, 1.000000000000000000, 0.9238795325112867385, 1.000000000000000000, 0.9238795325112867385, 1.000000000000000000, 0.9238795325112867385, 1.000000000000000000, 0.9238795325112867385, 1.000000000000000000, 0.9238795325112867385, 1.000000000000000000, 0.9238795325112867385, 1.000000000000000000, 0.9238795325112867385, 1.000000000000000000, 0.9238795325112867385, 1.000000000000000000, 0.9238795325112867385, 1.000000000000000000, 0.9238795325112867385, 1.000000000000000000, 0.9238795325112867385, 1.000000000000000000, 0.9238795325112867385, 1.000000000000000000, 0.9238795325112867385, 1.000000000000000000, 0.9238795325112867385, 1.000000000000000000, 0.9238795325112867385, 1.000000000000000000, 0.9238795325112867385, 1.000000000000000000, 0.9238795325112867385, 1.000000000000000000, 0.9238795325112867385, 1.000000000000000000, 0.9238795325112867385, 1.000000000000000000, 0.9238795325112867385, 1.000000000000000000, 0.9238795325112867385, 1.000000000000000000, 0.9238795325112867385, 1.000000000000000000, 0.9238795325112867385, 1.000000000000000000, 0.9238795325112867385, 1.000000000000000000, 0.9238795325112867385, 1.000000000000000000, 0.9238795325112867385, 1.000000000000000000, 0.9238795325112867385, 1.000000000000000000, 0.9238795325112867385, 1.000000000000000000, 0.9238795325112867385, 1.000000000000000000, 0.9238795325112867385, 1.000000000000000000, 0.9238795325112867385, 1.000000000000000000),
 ( 1.000000000000000000, 0.9238795325112867385, 1.000000000000000000, 0.9238795325112867385, 1.000000000000000000, 0.9238795325112867385, 1.000000000000000000, 0.9238795325112867385, 1.000000000000000000, 0.9238795325112867385, 1.000000000000000000, 0.9238795325112867385, 1.000000000000000000, 0.9238795325112867385, 1.000000000000000000, 0.9238795325112867385, 1.000000000000000000, 0.9238795325112867385, 1.000000000000000000, 0.9238795325112867385, 1.000000000000000000, 0.9238795325112867385, 1.000000000000000000, 0.9238795325112867385, 1.000000000000000000, 0.9238795325112867385, 1.000000000000000000, 0.9238795325112867385, 1.000000000000000000, 0.9238795325112867385, 1.000000000000000000, 0.9238795325112867385, 1.000000000000000000, 0.9238795325112867385, 1.000000000000000000, 0.9238795325112867385, 1.000000000000000000, 0.9238795325112867385, 1.000000000000000000, 0.9238795325112867385, 1.000000000000000000, 0.9238795325112867385, 1.000000000000000000, 0.9238795325112867385, 1.000000000000000000, 0.9238795325112867385, 1.000000000000000000, 0.9238795325112867385, 1.000000000000000000, 0.9238795325112867385, 1.000000000000000000, 0.9238795325112867385, 1.000000000000000000, 0.9238795325112867385, 1.000000000000000000, 0.9238795325112867385, 1.000000000000000000, 0.9238795325112867385, 1.000000000000000000, 0.9238795325112867385, 1.000000000000000000, 0.9238795325112867385, 1.000000000000000000, 0.9238795325112867385, 1.000000000000000000, 0.9238795325112867385, 1.000000000000000000, 0.9238795325112867385, 1.000000000000000000, 0.9238795325112867385, 1.000000000000000000, 0.9238795325112867385, 1.000000000000000000, 0.9238795325112867385, 1.000000000000000000, 0.9238795325112867385, 1.000000000000000000, 0.9238795325112867385, 1.000000000000000000, 0.9238795325112867385, 1.000000000000000000, 0.9238795325112867385, 1.000000000000000000, 0.9238795325112867385, 1.000000000000000000, 0.9238795325112867385, 1.000000000000000000, 0.9238795325112867385, 1.000000000000000000, 0.9238795325112867385, 1.000000000000000000, 0.9238795325112867385, 1.000000000000000000, 0.9238795325112867385, 1.000000000000000000, 0.9238795325112867385, 1.000000000000000000, 0.9238795325112867385, 1.000000000000000000, 0.9238795325112867385, 1.000000000000000000, 0.9238795325112867385, 1.000000000000000000, 0.9238795325112867385, 1.000000000000000000, 0.9238795325112867385, 1.000000000000000000, 0.9238795325112867385, 1.000000000000000000, 0.9238795325112867385, 1.000000000000000000, 0.9238795325112867385, 1.000000000000000000, 0.9238795325112867385, 1.000000000000000000, 0.9238795325112867385, 1.000000000000000000, 0.9238795325112867385, 1.000000000000000000, 0.9238795325112867385, 1.000000000000000000, 0.9238795325112867385, 1.000000000000000000, 0.9238795325112867385, 1.000000000000000000, 0.9238795325112867385, 1.000000000000000000, 0.9238795325112867385, 1.000000000000000000, 0.9238795325112867385, 1.000000000000000000, 0.9238795325112867385, 1.000000000000000000, 0.9238795325112867385, 1.000000000000000000, 0.9238795325112867385, 1.000000000000000000, 0.9238795325112867385, 1.000000000000000000, 0.9238795325112867385, 1.000000000000000000, 0.9238795325112867385, 1.000000000000000000, 0.9238795325112867385, 1.000000000000000000, 0.9238795325112867385, 1.000000000000000000, 0.9238795325112867385, 1.000000000000000000, 0.9238795325112867385, 1.000000000000000000, 0.9238795325112867385, 1.000000000000000000, 0.9238795325112867385, 1.000000000000000000, 0.9238795325112867385, 1.000000000000000000, 0.9238795325112867385, 1.000000000000000000, 0.9238795325112867385, 1.000000000000000000, 0.9238795325112867385, 1.000000000000000000, 0.9238795325112867385, 1.000000000000000000, 0.9238795325112867385, 1.000000000000000000, 0.9238795325112867385, 1.000000000000000000, 0.9238795325112867385, 1.000000000000000000, 0.9238795325112867385, 1.000000000000000000, 0.9238795325112867385, 1.000000000000000000, 0.9238795325112867385, 1.000000000000000000, 0.9238795325112867385, 1.000000000000000000, 0.9238795325112867385, 1.000000000000000000) ) ) 
 REPRESENTATION_ITEM ( '' )  SURFACE ( )  );
#18626 = CARTESIAN_POINT ( 'NONE',  ( 0.000000000000000000, 0.000000000000000000, 1.326383476483184332 ) ) ;
#18627 = CARTESIAN_POINT ( 'NONE',  ( -8.379073922441706732E-07, 4.293833316950179224, 0.3119999999988748440 ) ) ;
#18628 = CARTESIAN_POINT ( 'NONE',  ( 1.973001146175422216, 2.291712385858714729, -1.876529041877834203 ) ) ;
#18629 = CARTESIAN_POINT ( 'NONE',  ( -0.3119999999999999996, 4.602861111111111292, -0.1292346314604056468 ) ) ;
#18630 = CARTESIAN_POINT ( 'NONE',  ( 0.1993543840281267465, 3.818138888964754507, 0.1993543840281266633 ) ) ;
#18631 = CARTESIAN_POINT ( 'NONE',  ( 0.4199999999999995959, 0.04999999999999921868, -0.02499999999999958505 ) ) ;
#18632 = LINE ( 'NONE', #11203, #15514 ) ;
#18633 = CARTESIAN_POINT ( 'NONE',  ( 2.055580586463031434, 2.740000000000000213, -2.936000000000001720 ) ) ;
#18634 = FACE_OUTER_BOUND ( 'NONE', #19905, .T. ) ;
#18635 = CARTESIAN_POINT ( 'NONE',  ( -0.3856318672988793272, -0.3186212149721687203, 0.4002893343786020908 ) ) ;
#18636 = AXIS2_PLACEMENT_3D ( 'NONE', #21849, #12366, #19783 ) ;
#18637 = CARTESIAN_POINT ( 'NONE',  ( 0.2667111700250733852, 4.645955859489413697, -0.1672198252236019589 ) ) ;
#18638 = EDGE_CURVE ( 'NONE', #9500, #20728, #4913, .T. ) ;
#18639 = CARTESIAN_POINT ( 'NONE',  ( 0.2764156081756483641, -0.1144950937579611167, 0.2793055555555589153 ) ) ;
#18640 = ADVANCED_FACE ( 'NONE', ( #17969 ), #15683, .F. ) ;
#18641 = CARTESIAN_POINT ( 'NONE',  ( -0.4687500000000003886, -0.2598076211353319009, 0.3779506566538942125 ) ) ;
#18642 = DIRECTION ( 'NONE',  ( -0.000000000000000000, -1.000000000000000000, -0.000000000000000000 ) ) ;
#18643 = VERTEX_POINT ( 'NONE', #5393 ) ;
#18644 = CARTESIAN_POINT ( 'NONE',  ( -0.2923287055106771337, 0.2687499999024575703, 0.2123892367102619971 ) ) ;
#18645 = CARTESIAN_POINT ( 'NONE',  ( -0.2819296736111110979, 0.2854166665908000611, -3.452642723725051716E-17 ) ) ;
#18646 = CARTESIAN_POINT ( 'NONE',  ( 0.1571321947316088596, 3.872627114028808659, -0.2726197584672552243 ) ) ;
#18647 = CARTESIAN_POINT ( 'NONE',  ( 0.2727677001506427223, 0.6283691918605152082, -1.089234312191128540 ) ) ;
#18648 = CC_DESIGN_PERSON_AND_ORGANIZATION_ASSIGNMENT ( #19780, #4542, ( #9980 ) ) ;
#18649 = CARTESIAN_POINT ( 'NONE',  ( 1.726321361862525858E-17, 0.6048611110352445364, -0.2819296736111110979 ) ) ;
#18650 = CARTESIAN_POINT ( 'NONE',  ( -0.1144950937579609779, 0.2764156081756484196, -0.08180555555555503455 ) ) ;
#18651 = CARTESIAN_POINT ( 'NONE',  ( 1.573500000000000343, 0.5250000000000000222, -0.1650000000000001465 ) ) ;
#18652 = DIRECTION ( 'NONE',  ( -0.000000000000000000, -1.000000000000000000, -0.000000000000000000 ) ) ;
#18653 = CARTESIAN_POINT ( 'NONE',  ( 0.2206173157302028232, -0.03055555555555588762, -0.2206173157302028232 ) ) ;
#18654 = CARTESIAN_POINT ( 'NONE',  ( 0.1292346314604058410, 5.068138888888887195, 0.3119999999999998885 ) ) ;
#18655 = VECTOR ( 'NONE', #10707, 39.37007874015748143 ) ;
#18656 = CARTESIAN_POINT ( 'NONE',  ( 0.2923287055106771337, 0.3044642856167432687, -0.2123892367102620249 ) ) ;
#18657 = CARTESIAN_POINT ( 'NONE',  ( -0.1993543840281266355, 4.207027777853643791, 0.1993543840281267465 ) ) ;
#18658 = CARTESIAN_POINT ( 'NONE',  ( 0.3119999999999999996, 0.1222222220704892864, 0.000000000000000000 ) ) ;
#18659 = DIRECTION ( 'NONE',  ( 1.000000000000000000, 0.000000000000000000, 0.000000000000000000 ) ) ;
#18660 = ORIENTED_EDGE ( 'NONE', *, *, #19008, .F. ) ;
#18661 = LINE ( 'NONE', #14413, #7380 ) ;
#18662 = CARTESIAN_POINT ( 'NONE',  ( 0.2819296736111110424, 5.050777777853643791, -0.1167790944451423396 ) ) ;
#18663 = CARTESIAN_POINT ( 'NONE',  ( -0.2854617896337424132, 5.152931539520130499, -0.09929655918317221996 ) ) ;
#18664 =( CONVERSION_BASED_UNIT ( 'INCH', #11238 ) LENGTH_UNIT ( ) NAMED_UNIT ( #736 ) );
#18665 = CARTESIAN_POINT ( 'NONE',  ( 0.000000000000000000, 3.700000000000000622, -0.4000000000000000222 ) ) ;
#18666 = CARTESIAN_POINT ( 'NONE',  ( 0.06335377612981443751, 0.1696876529123872990, 0.4000000000000000222 ) ) ;
#18667 = CIRCLE ( 'NONE', #10124, 0.01875000000000000625 ) ;
#18668 = CARTESIAN_POINT ( 'NONE',  ( -1.726321361862525858E-17, 4.616750000075865223, -0.2819296736111110979 ) ) ;
#18669 = PERSON_AND_ORGANIZATION ( #18449, #21280 ) ;
#18670 = CARTESIAN_POINT ( 'NONE',  ( -0.4621660567954124499, 0.2744341800641371676, 0.05971082423030620728 ) ) ;
#18671 = CARTESIAN_POINT ( 'NONE',  ( -1.910449006669871087E-17, 4.925777777777777366, -0.3119999999999999996 ) ) ;
#18672 = CARTESIAN_POINT ( 'NONE',  ( -0.2819296736111110979, 0.5770833332574666352, -3.452642723725051716E-17 ) ) ;
#18673 = ORIENTED_EDGE ( 'NONE', *, *, #17169, .F. ) ;
#18674 = CARTESIAN_POINT ( 'NONE',  ( -0.1993543840281267465, 0.3062499999241333759, 0.1993543840281266633 ) ) ;
#18675 = DIRECTION ( 'NONE',  ( 0.03777542905056541916, -0.9971419496943164651, -0.06542896239329260011 ) ) ;
#18676 = CARTESIAN_POINT ( 'NONE',  ( -0.4000000000000000222, 0.3589285712334865375, 0.1299678784931624920 ) ) ;
#18677 = CARTESIAN_POINT ( 'NONE',  ( 0.1236067977499789861, 0.1999999999999999278, -0.3804226065180614236 ) ) ;
#18678 = CARTESIAN_POINT ( 'NONE',  ( 0.3155070326520292290, 0.1306872919485615736, 0.03798611111111236532 ) ) ;
#18679 = ADVANCED_FACE ( 'NONE', ( #10650 ), #3443, .T. ) ;
#18680 = CARTESIAN_POINT ( 'NONE',  ( -0.01848103877824596938, -0.5441716683897390716, 0.04413116910601656145 ) ) ;
#18681 = FACE_OUTER_BOUND ( 'NONE', #19354, .T. ) ;
#18682 = CARTESIAN_POINT ( 'NONE',  ( -5.178964085587577574E-17, 0.3548611110352444808, 0.2819296736111110979 ) ) ;
#18683 = CARTESIAN_POINT ( 'NONE',  ( 0.2819296736111110979, 0.03541666659080003332, 0.000000000000000000 ) ) ;
#18684 = CARTESIAN_POINT ( 'NONE',  ( -0.1993543840281266910, 4.193138888964754507, -0.1993543840281266910 ) ) ;
#18685 = CARTESIAN_POINT ( 'NONE',  ( 0.1236067977499789861, 0.04821428551920092093, -0.3804226065180614236 ) ) ;
#18686 = CARTESIAN_POINT ( 'NONE',  ( -0.2819296736111110979, 5.200083333409199149, 0.000000000000000000 ) ) ;
#18687 = CARTESIAN_POINT ( 'NONE',  ( 5.178964085587577574E-17, 4.477861111186976828, 0.2819296736111110979 ) ) ;
#18688 = CIRCLE ( 'NONE', #6621, 0.01874999999999999237 ) ;
#18689 = CARTESIAN_POINT ( 'NONE',  ( -0.3125000000000000000, 0.000000000000000000, 1.326383476483184332 ) ) ;
#18690 = VECTOR ( 'NONE', #9419, 39.37007874015747433 ) ;
#18691 = ORIENTED_EDGE ( 'NONE', *, *, #5432, .F. ) ;
#18692 = CARTESIAN_POINT ( 'NONE',  ( 0.1831830759718832136, 3.927233054027901460, -0.2570004728143698847 ) ) ;
#18693 = CARTESIAN_POINT ( 'NONE',  ( 0.2206173157302027954, 4.148000000151731648, -0.2206173157302028232 ) ) ;
#18694 = CARTESIAN_POINT ( 'NONE',  ( 0.000000000000000000, 0.06249999999999967387, 0.3119999999999999996 ) ) ;
#18695 = EDGE_LOOP ( 'NONE', ( #21944, #15488, #17499, #19172 ) ) ;
#18696 = EDGE_CURVE ( 'NONE', #1943, #21079, #23912, .T. ) ;
#18697 = EDGE_CURVE ( 'NONE', #6276, #1106, #8810, .T. ) ;
#18698 = EDGE_CURVE ( 'NONE', #22988, #8072, #16382, .T. ) ;
#18699 = VERTEX_POINT ( 'NONE', #21859 ) ;
#18700 = CALENDAR_DATE ( 2026, 7, 10 ) ;
#18701 = CARTESIAN_POINT ( 'NONE',  ( -0.2774634594257631148, -0.1150700753241015728, 0.4115780677775827678 ) ) ;
#18702 = AXIS2_PLACEMENT_3D ( 'NONE', #3536, #1823, #7556 ) ;
#18703 = CARTESIAN_POINT ( 'NONE',  ( -0.1378975025881151173, 4.845326366584603583, 0.2798720040862737735 ) ) ;
#18704 = CARTESIAN_POINT ( 'NONE',  ( 2.345681073014820761, 0.05000000000000028727, -2.986000000000000210 ) ) ;
#18705 = ORIENTED_EDGE ( 'NONE', *, *, #226, .F. ) ;
#18706 = B_SPLINE_CURVE_WITH_KNOTS ( 'NONE', 3,
 ( #17442, #9772, #20858, #2454 ),
 .UNSPECIFIED., .F., .F.,
 ( 4, 4 ),
 ( 0.000000000000000000, 0.002245614500286350051 ),
 .UNSPECIFIED. ) ;
#18707 = CARTESIAN_POINT ( 'NONE',  ( -0.3119999999999999996, 0.4312499998482670627, 0.1292346314604056190 ) ) ;
#18708 = AXIS2_PLACEMENT_3D ( 'NONE', #9822, #19555, #8332 ) ;
#18709 = LINE ( 'NONE', #2007, #5884 ) ;
#18710 = CARTESIAN_POINT ( 'NONE',  ( 0.2262030867566338643, 4.745356984526616806, 0.2181069733381811870 ) ) ;
#18711 = CARTESIAN_POINT ( 'NONE',  ( -0.3613381517857144343, 0.1044642856167432993, 0.1174058825155740171 ) ) ;
#18712 = CARTESIAN_POINT ( 'NONE',  ( 0.3120465040799779710, 3.975505242139018680, -0.04045383393106066761 ) ) ;
#18713 = EDGE_CURVE ( 'NONE', #18597, #14213, #1365, .T. ) ;
#18714 = ORIENTED_EDGE ( 'NONE', *, *, #6455, .T. ) ;
#18715 = CARTESIAN_POINT ( 'NONE',  ( 2.326421213736078119E-17, 0.1008928570453146989, -0.3799334167787516980 ) ) ;
#18716 = DIRECTION ( 'NONE',  ( -1.000000000000000000, 0.000000000000000000, 0.000000000000000000 ) ) ;
#18717 = CARTESIAN_POINT ( 'NONE',  ( -0.3115938335747658328, 4.668094915020961189, -0.02818765380693593822 ) ) ;
#18718 = CARTESIAN_POINT ( 'NONE',  ( -0.1993543840281266910, 4.234805555631421470, -0.1993543840281266910 ) ) ;
#18719 = CARTESIAN_POINT ( 'NONE',  ( -0.4687500000000004441, -0.08745052389986680830, 0.08858773447093010178 ) ) ;
#18720 = CARTESIAN_POINT ( 'NONE',  ( 0.3101024306885722948, -0.3622281555308699552, 0.08858850926231194578 ) ) ;
#18721 = CARTESIAN_POINT ( 'NONE',  ( -0.3119999999999999996, 3.880638888888887639, -0.1292346314604056468 ) ) ;
#18722 = LINE ( 'NONE', #2140, #6085 ) ;
#18723 = CARTESIAN_POINT ( 'NONE',  ( 0.3119999999999999996, 4.641055555707287006, -3.820898013339742174E-17 ) ) ;
#18724 = CARTESIAN_POINT ( 'NONE',  ( -0.2819296736111110424, 5.148000000075865223, 0.1167790944451424923 ) ) ;
#18725 = CIRCLE ( 'NONE', #21834, 1.243000000000000105 ) ;
#18726 = CIRCLE ( 'NONE', #8201, 0.01874999999999999931 ) ;
#18727 = CARTESIAN_POINT ( 'NONE',  ( 9.184850993605150903E-17, 0.9099999999999988098, -0.7500000000000001110 ) ) ;
#18728 = ORIENTED_EDGE ( 'NONE', *, *, #2364, .T. ) ;
#18729 = CARTESIAN_POINT ( 'NONE',  ( -0.1116596296178199582, 0.2294642856167432854, -0.3436530038418508792 ) ) ;
#18730 = CARTESIAN_POINT ( 'NONE',  ( 0.1702787520999720638, 0.03957802798364115637, -0.2338844550317653315 ) ) ;
#18731 = EDGE_CURVE ( 'NONE', #11776, #2004, #8190, .T. ) ;
#18732 = ORIENTED_EDGE ( 'NONE', *, *, #1891, .F. ) ;
#18733 = APPROVAL_ROLE ( '' ) ;
#18734 = CARTESIAN_POINT ( 'NONE',  ( -0.3155070326520292845, 1.931923388228935888E-17, 0.3990972222222267662 ) ) ;
#18735 = CARTESIAN_POINT ( 'NONE',  ( -0.2819296736111110424, 5.127166666742532186, -0.1167790944451423119 ) ) ;
#18736 = CARTESIAN_POINT ( 'NONE',  ( 0.1167790944451424506, 3.884111111186977272, 0.2819296736111110424 ) ) ;
#18737 = CARTESIAN_POINT ( 'NONE',  ( 0.1551925990475264694, 4.409532269935922066, 0.2718825043972741828 ) ) ;
#18738 = EDGE_CURVE ( 'NONE', #20523, #15341, #2110, .T. ) ;
#18739 = LINE ( 'NONE', #10947, #11427 ) ;
#18740 = VECTOR ( 'NONE', #2690, 39.37007874015748143 ) ;
#18741 = CARTESIAN_POINT ( 'NONE',  ( 0.1954553509668046640, -0.1954553509668047195, 0.1091666666666687158 ) ) ;
#18742 = CARTESIAN_POINT ( 'NONE',  ( -5.178964085587577574E-17, 0.5909722221463555858, 0.2819296736111110979 ) ) ;
#18743 = CARTESIAN_POINT ( 'NONE',  ( -0.1144950937579609779, 0.2764156081756484196, 0.1404166666666689378 ) ) ;
#18744 = CARTESIAN_POINT ( 'NONE',  ( 0.2819296736111110979, 4.891055555631421470, 0.1167790944451422425 ) ) ;
#18745 = CARTESIAN_POINT ( 'NONE',  ( -0.01848103877826416663, -0.5441716683897284135, 0.04413116910602139092 ) ) ;
#18746 = CARTESIAN_POINT ( 'NONE',  ( 5.178964085587577574E-17, 4.811194444520309865, 0.2819296736111110979 ) ) ;
#18747 = DIRECTION ( 'NONE',  ( -0.000000000000000000, -1.000000000000000000, -0.000000000000000000 ) ) ;
#18748 = CARTESIAN_POINT ( 'NONE',  ( 5.731347020009612645E-17, 5.064666666666665762, 0.3119999999999999996 ) ) ;
#18749 = DIRECTION ( 'NONE',  ( -0.000000000000000000, -1.000000000000000000, -0.000000000000000000 ) ) ;
#18750 = CARTESIAN_POINT ( 'NONE',  ( 1.728575740896261204, 2.453214835500605595, -2.009490367722004400 ) ) ;
#18751 = CARTESIAN_POINT ( 'NONE',  ( 0.1292346314604058410, 4.457027777777777366, 0.3119999999999998885 ) ) ;
#18752 = CARTESIAN_POINT ( 'NONE',  ( -0.3999999999999999667, 0.2892857142857141461, -0.1299678784931626030 ) ) ;
#18753 = DIRECTION ( 'NONE',  ( 1.000000000000000000, 0.000000000000000000, 0.000000000000000000 ) ) ;
#18754 = CARTESIAN_POINT ( 'NONE',  ( 1.573500000000000343, -3.414809992080329023E-17, -0.9499999999999999556 ) ) ;
#18755 = CARTESIAN_POINT ( 'NONE',  ( -0.1052696321117038564, 3.735245827680147013, 0.2937044510672804365 ) ) ;
#18756 = CARTESIAN_POINT ( 'NONE',  ( 0.3091804297555219017, 4.584330404083684307, 0.04228285750231519646 ) ) ;
#18757 = ORIENTED_EDGE ( 'NONE', *, *, #2836, .T. ) ;
#18758 = CARTESIAN_POINT ( 'NONE',  ( -0.1179188671565439273, 4.123723453325901289, 0.2893754189311016356 ) ) ;
#18759 = CARTESIAN_POINT ( 'NONE',  ( -0.1166234456863258218, 4.111524471938507119, -2.868834514064774854 ) ) ;
#18760 = CARTESIAN_POINT ( 'NONE',  ( 0.000000000000000000, 0.3155070326520292845, -0.1147916666666661950 ) ) ;
#18761 = DIRECTION ( 'NONE',  ( -0.8660254037844433705, 0.000000000000000000, 0.4999999999999917843 ) ) ;
#18762 = CARTESIAN_POINT ( 'NONE',  ( 0.3010013639763466919, 5.147262939741143128, -0.03641029953439574307 ) ) ;
#18763 = EDGE_CURVE ( 'NONE', #549, #10191, #16513, .T. ) ;
#18764 = VERTEX_POINT ( 'NONE', #8688 ) ;
#18765 = CARTESIAN_POINT ( 'NONE',  ( -0.2923287055106771337, 0.3973214284738861291, -0.2123892367102620804 ) ) ;
#18766 = CARTESIAN_POINT ( 'NONE',  ( 0.2819296736111110979, 0.3687499999241333759, 0.000000000000000000 ) ) ;
#18767 = CARTESIAN_POINT ( 'NONE',  ( 0.3038812257567455322, 3.865502245511798662, -0.08165866421004353004 ) ) ;
#18768 = CARTESIAN_POINT ( 'NONE',  ( 0.2082036761074528841, 0.7085065112206522242, -1.081619176768333412 ) ) ;
#18769 = CARTESIAN_POINT ( 'NONE',  ( 0.4226370775080297015, 0.2972562468964968785, 0.3901966308178841936 ) ) ;
#18770 = CARTESIAN_POINT ( 'NONE',  ( 0.1144950937579609085, -0.2764156081756484751, 0.1681944444444469222 ) ) ;
#18771 = DIRECTION ( 'NONE',  ( -1.000000000000000000, 0.000000000000000000, 0.000000000000000000 ) ) ;
#18772 = CARTESIAN_POINT ( 'NONE',  ( 0.3119999999999999996, 4.359805555555555046, -0.1292346314604056745 ) ) ;
#18773 = CARTESIAN_POINT ( 'NONE',  ( 0.3119999999999998885, 0.2923611111111107386, 0.1292346314604058410 ) ) ;
#18774 = CARTESIAN_POINT ( 'NONE',  ( -0.3119999999999999996, 5.217444444444443441, 0.000000000000000000 ) ) ;
#18775 = B_SPLINE_CURVE_WITH_KNOTS ( 'NONE', 3,
 ( #20726, #11714, #5736, #4023 ),
 .UNSPECIFIED., .F., .F.,
 ( 4, 4 ),
 ( 0.08935694927272852528, 0.1543853174178340670 ),
 .UNSPECIFIED. ) ;
#18776 = CARTESIAN_POINT ( 'NONE',  ( -0.1993543840281266355, 4.262583333409199149, 0.1993543840281267465 ) ) ;
#18777 = CARTESIAN_POINT ( 'NONE',  ( 0.000000000000000000, 0.02999999999999995379, 0.000000000000000000 ) ) ;
#18778 = CARTESIAN_POINT ( 'NONE',  ( 3.061616997868383018E-17, 0.4987679491924311148, -0.2500000000000000000 ) ) ;
#18779 = ORIENTED_EDGE ( 'NONE', *, *, #18402, .T. ) ;
#18780 = ORIENTED_EDGE ( 'NONE', *, *, #4831, .F. ) ;
#18781 = CARTESIAN_POINT ( 'NONE',  ( -0.3125000000000000000, 1.913510623667739771E-17, 0.1230555555555578606 ) ) ;
#18782 = CARTESIAN_POINT ( 'NONE',  ( 0.2819296736111110424, 4.995222222298087544, -0.1167790944451423396 ) ) ;
#18783 = VECTOR ( 'NONE', #12553, 39.37007874015748143 ) ;
#18784 = CARTESIAN_POINT ( 'NONE',  ( 0.000000000000000000, 0.3125000000000000000, -0.001944444444443116891 ) ) ;
#18785 =( NAMED_UNIT ( * ) SI_UNIT ( $, .STERADIAN. ) SOLID_ANGLE_UNIT ( ) );
#18786 = CARTESIAN_POINT ( 'NONE',  ( 0.4581189881604794123, 0.2644951211353319120, 0.3941886329748525153 ) ) ;
#18787 = CC_DESIGN_DATE_AND_TIME_ASSIGNMENT ( #10490, #23387, ( #14477 ) ) ;
#18788 = CARTESIAN_POINT ( 'NONE',  ( 1.910449006669871087E-17, 0.6361111109593781121, -0.3119999999999999996 ) ) ;
#18789 = CARTESIAN_POINT ( 'NONE',  ( -0.1167790944451423119, 4.731333333409199149, -0.2819296736111110979 ) ) ;
#18790 = CALENDAR_DATE ( 2026, 7, 10 ) ;
#18791 = CARTESIAN_POINT ( 'NONE',  ( -0.1926153850652713162, 4.049733122821375098, -0.2454647334727473040 ) ) ;
#18792 = CARTESIAN_POINT ( 'NONE',  ( 0.1954553509668047195, 0.1954553509668046085, 0.07444444444444621445 ) ) ;
#18793 = CARTESIAN_POINT ( 'NONE',  ( -5.178964085587577574E-17, 0.4798611110352444253, 0.2819296736111110979 ) ) ;
#18794 = ORIENTED_EDGE ( 'NONE', *, *, #16033, .T. ) ;
#18795 = CARTESIAN_POINT ( 'NONE',  ( 0.1993543840281266910, 0.2229166665908000333, -0.1993543840281266910 ) ) ;
#18796 = DIRECTION ( 'NONE',  ( 0.000000000000000000, 0.000000000000000000, 1.000000000000000000 ) ) ;
#18797 = CARTESIAN_POINT ( 'NONE',  ( -0.3124999999999993894, -0.1294417382415926909, 0.1751388888888912587 ) ) ;
#18798 = CARTESIAN_POINT ( 'NONE',  ( 0.3999999999999999667, 0.1821428571428570231, 0.1299678784931626307 ) ) ;
#18799 = CARTESIAN_POINT ( 'NONE',  ( -3.863846776457871776E-17, -0.3155070326520292845, 0.02062500000000112854 ) ) ;
#18800 = VECTOR ( 'NONE', #19434, 39.37007874015748143 ) ;
#18801 = CARTESIAN_POINT ( 'NONE',  ( 0.8043248696826207356, 2.291712385858714285, -0.5923223533918536843 ) ) ;
#18802 = DIRECTION ( 'NONE',  ( 0.000000000000000000, 0.000000000000000000, -1.000000000000000000 ) ) ;
#18803 = CARTESIAN_POINT ( 'NONE',  ( 0.1167790944451423119, 0.3236111110352444808, -0.2819296736111110979 ) ) ;
#18804 = CARTESIAN_POINT ( 'NONE',  ( 0.9253895857510197054, 2.315961009048385755, -1.333958623133626009 ) ) ;
#18805 = CARTESIAN_POINT ( 'NONE',  ( -0.1993543840281266910, 4.304250000075866112, -0.1993543840281266910 ) ) ;
#18806 = CARTESIAN_POINT ( 'NONE',  ( -0.1236067977499790416, 0.1553571426620580509, 0.3804226065180614236 ) ) ;
#18807 = CARTESIAN_POINT ( 'NONE',  ( -0.1993543840281266910, 4.915361111186976828, -0.1993543840281266910 ) ) ;
#18808 = CARTESIAN_POINT ( 'NONE',  ( -0.1167790944451423535, 4.474388888964753619, 0.2819296736111110979 ) ) ;
#18809 = DIRECTION ( 'NONE',  ( -0.000000000000000000, -1.000000000000000000, -0.000000000000000000 ) ) ;
#18810 = ORIENTED_EDGE ( 'NONE', *, *, #2627, .F. ) ;
#18811 = CARTESIAN_POINT ( 'NONE',  ( -0.01848103877824615326, 0.5441716683897390716, 0.04413116910601658227 ) ) ;
#18812 = CARTESIAN_POINT ( 'NONE',  ( 0.2206173157302027954, 3.981333333485065573, -0.2206173157302028232 ) ) ;
#18813 =( BOUNDED_CURVE ( )  B_SPLINE_CURVE ( 2, ( #2718, #647, #15527, #4182, #22948, #19061, #10170, #6250, #13711, #12007, #6005, #21131, #2604 ),
 .UNSPECIFIED., .F., .T. ) 
 B_SPLINE_CURVE_WITH_KNOTS ( ( 3, 2, 2, 2, 2, 2, 3 ),
 ( 0.8214285714285715079, 0.8285714285714286254, 0.8428571428571428603, 0.8571428571428570953, 0.8714285714285714413, 0.8857142857142856762, 0.8928571428571429047 ),
 .UNSPECIFIED. ) 
 CURVE ( )  GEOMETRIC_REPRESENTATION_ITEM ( )  RATIONAL_B_SPLINE_CURVE ( ( 0.9755282581475768211, 0.9755282581475769321, 1.000000000000000000, 0.9510565162951535312, 1.000000000000000000, 0.9510565162951535312, 1.000000000000000000, 0.9510565162951535312, 1.000000000000000000, 0.9510565162951535312, 1.000000000000000000, 0.9755282581475765991, 0.9755282581475768211 ) ) 
 REPRESENTATION_ITEM ( '' )  );
#18814 =( BOUNDED_CURVE ( )  B_SPLINE_CURVE ( 2, ( #10163, #21248, #12356, #19775, #23531, #21726, #12473, #19893, #3184 ),
 .UNSPECIFIED., .F., .F. ) 
 B_SPLINE_CURVE_WITH_KNOTS ( ( 3, 2, 2, 2, 3 ),
 ( 0.7946428571428569843, 0.7991071428571429047, 0.8035714285714286031, 0.8080357142857144126, 0.8125000000000002220 ),
 .UNSPECIFIED. ) 
 CURVE ( )  GEOMETRIC_REPRESENTATION_ITEM ( )  RATIONAL_B_SPLINE_CURVE ( ( 1.000000000000001998, 0.9238795325112848511, 1.000000000000000000, 0.9238795325112867385, 1.000000000000000000, 0.9238795325112867385, 1.000000000000000000, 0.9238795325112829637, 1.000000000000003775 ) ) 
 REPRESENTATION_ITEM ( '' )  );
#18815 = CARTESIAN_POINT ( 'NONE',  ( 1.951887815886574673, 2.740000000000000213, -1.126922955930076409 ) ) ;
#18816 = VECTOR ( 'NONE', #3496, 39.37007874015748143 ) ;
#18817 = EDGE_CURVE ( 'NONE', #21481, #13516, #22733, .T. ) ;
#18818 = CARTESIAN_POINT ( 'NONE',  ( -0.01239990016104709422, -0.3069330571738640989, -0.09589278090496755613 ) ) ;
#18819 = ORIENTED_EDGE ( 'NONE', *, *, #3643, .F. ) ;
#18820 = B_SPLINE_CURVE_WITH_KNOTS ( 'NONE', 3,
 ( #14718, #1653, #7150, #9217, #24078, #13138, #18719, #22132, #3361, #21894 ),
 .UNSPECIFIED., .F., .F.,
 ( 4, 2, 2, 2, 4 ),
 ( 0.000000000000000000, 0.003321853704944119183, 0.006643707409888238366, 0.009965561114832356682, 0.01328741481977647673 ),
 .UNSPECIFIED. ) ;
#18821 = COORDINATED_UNIVERSAL_TIME_OFFSET ( 0, 0, .AHEAD. ) ;
#18822 = ORIENTED_EDGE ( 'NONE', *, *, #3105, .F. ) ;
#18823 = CARTESIAN_POINT ( 'NONE',  ( 6.614309848781084774E-13, 0.03242967361111062652, 0.2819296736111109869 ) ) ;
#18824 = CARTESIAN_POINT ( 'NONE',  ( 0.000000000000000000, 5.072999999999999510, 0.000000000000000000 ) ) ;
#18825 = ORIENTED_EDGE ( 'NONE', *, *, #11935, .T. ) ;
#18826 = CARTESIAN_POINT ( 'NONE',  ( -0.1292346314604058410, 0.4937499998482670627, 0.3119999999999998885 ) ) ;
#18827 = VERTEX_POINT ( 'NONE', #20751 ) ;
#18828 = CARTESIAN_POINT ( 'NONE',  ( -1.144996993574672217, 3.066692553488282957, 2.183691821209530648 ) ) ;
#18829 = CARTESIAN_POINT ( 'NONE',  ( 0.3100543665041115560, 0.3622559054007069013, 0.4143868288130764799 ) ) ;
#18830 = CARTESIAN_POINT ( 'NONE',  ( 0.4500000000000003442, 0.2598076211353318454, 0.3779506566538943235 ) ) ;
#18831 = CARTESIAN_POINT ( 'NONE',  ( 0.1116596296178199027, 0.1223214284738861762, 0.3436530038418508792 ) ) ;
#18832 = CARTESIAN_POINT ( 'NONE',  ( 0.3037978522088217725, 3.972042276961438745, 0.08195363556016189988 ) ) ;
#18833 = EDGE_LOOP ( 'NONE', ( #11099, #5650, #7136 ) ) ;
#18834 = CARTESIAN_POINT ( 'NONE',  ( -6.979263641208234666E-17, 0.2080357141881718774, 0.3799334167787516980 ) ) ;
#18835 = ORIENTED_EDGE ( 'NONE', *, *, #21901, .F. ) ;
#18836 = DIRECTION ( 'NONE',  ( -0.000000000000000000, -1.000000000000000000, -0.000000000000000000 ) ) ;
#18837 = CARTESIAN_POINT ( 'NONE',  ( -0.2297610394007475187, 4.675419736397950388, 0.2110789231160656865 ) ) ;
#18838 = AXIS2_PLACEMENT_3D ( 'NONE', #1260, #19793, #7233 ) ;
#18839 = CARTESIAN_POINT ( 'NONE',  ( 0.1993543840281267465, 3.929250000075865668, 0.1993543840281266633 ) ) ;
#18840 = CARTESIAN_POINT ( 'NONE',  ( 0.1311301917775922199, 5.040099063258902667, -0.2838626894904294207 ) ) ;
#18841 = CARTESIAN_POINT ( 'NONE',  ( -0.3119999999999999996, 4.828555555555555046, 0.000000000000000000 ) ) ;
#18842 = CARTESIAN_POINT ( 'NONE',  ( -0.1292346314604056745, 3.929249999999998799, -0.3119999999999999996 ) ) ;
#18843 = EDGE_CURVE ( 'NONE', #17116, #20229, #22698, .T. ) ;
#18844 = CARTESIAN_POINT ( 'NONE',  ( 5.731347020009612645E-17, 4.793833333485065573, 0.3119999999999999996 ) ) ;
#18845 = CARTESIAN_POINT ( 'NONE',  ( 0.1993543840281266633, 4.901472222298088433, -0.1993543840281266910 ) ) ;
#18846 = VERTEX_POINT ( 'NONE', #9295 ) ;
#18847 = CARTESIAN_POINT ( 'NONE',  ( -1.726321361862525858E-17, 4.394527777853643791, -0.2819296736111110979 ) ) ;
#18848 = LINE ( 'NONE', #7511, #22201 ) ;
#18849 = EDGE_LOOP ( 'NONE', ( #12351, #22005, #6634, #15958 ) ) ;
#18850 = CARTESIAN_POINT ( 'NONE',  ( 2.326421213736078119E-17, 0.1544642856167433020, -0.3799334167787516980 ) ) ;
#18851 = EDGE_CURVE ( 'NONE', #4238, #7496, #5562, .T. ) ;
#18852 = VERTEX_POINT ( 'NONE', #15152 ) ;
#18853 = ORIENTED_EDGE ( 'NONE', *, *, #8254, .F. ) ;
#18854 = SECURITY_CLASSIFICATION_LEVEL ( 'unclassified' ) ;
#18855 = CIRCLE ( 'NONE', #932, 0.7700000000000013500 ) ;
#18856 = CARTESIAN_POINT ( 'NONE',  ( 0.000000000000000000, 3.700000000000000622, 0.000000000000000000 ) ) ;
#18857 = CARTESIAN_POINT ( 'NONE',  ( -0.1993543840281266910, 5.123694444520309865, -0.1993543840281266910 ) ) ;
#18858 = CARTESIAN_POINT ( 'NONE',  ( -0.1993543840281266910, 3.915361111186976384, -0.1993543840281266910 ) ) ;
#18859 = APPLICATION_CONTEXT ( 'configuration controlled 3d designs of mechanical parts and assemblies' ) ;
#18860 = CARTESIAN_POINT ( 'NONE',  ( 0.1054935783943683481, 4.429683660412986335, -0.2936247782397201633 ) ) ;
#18861 = DIRECTION ( 'NONE',  ( -0.000000000000000000, -1.000000000000000000, -0.000000000000000000 ) ) ;
#18862 = CARTESIAN_POINT ( 'NONE',  ( 0.000000000000000000, 0.2764156081756484196, 0.2411111111111142458 ) ) ;
#18863 = CARTESIAN_POINT ( 'NONE',  ( 0.1993543840281266355, 0.5979166665908001166, 0.1993543840281267465 ) ) ;
#18864 = CARTESIAN_POINT ( 'NONE',  ( -0.2764156081756484196, 1.692557448933383907E-17, 0.3730555555555596925 ) ) ;
#18865 = CARTESIAN_POINT ( 'NONE',  ( -1.726321361862525858E-17, 4.852861111186976828, -0.2819296736111110979 ) ) ;
#18866 = CARTESIAN_POINT ( 'NONE',  ( -7.000945310522701902E-17, 0.4446428569477722803, 0.3999999999999999667 ) ) ;
#18867 = CARTESIAN_POINT ( 'NONE',  ( -0.2819296736111110424, 4.911888888964754507, 0.1167790944451424923 ) ) ;
#18868 = DIRECTION ( 'NONE',  ( 0.000000000000000000, 0.000000000000000000, -1.000000000000000000 ) ) ;
#18869 = EDGE_CURVE ( 'NONE', #5628, #9027, #12964, .T. ) ;
#18870 = DIRECTION ( 'NONE',  ( 0.000000000000000000, 0.000000000000000000, -1.000000000000000000 ) ) ;
#18871 = CARTESIAN_POINT ( 'NONE',  ( -0.3917008400274854529, -3.329947049564607987E-18, 0.07871827179061374746 ) ) ;
#18872 = DIRECTION ( 'NONE',  ( -0.000000000000000000, 1.000000000000000000, -0.000000000000000000 ) ) ;
#18873 = ADVANCED_FACE ( 'NONE', ( #11133 ), #14620, .F. ) ;
#18874 = CARTESIAN_POINT ( 'NONE',  ( 0.2206173157302027954, 4.529944444444443441, -0.2206173157302028232 ) ) ;
#18875 = EDGE_CURVE ( 'NONE', #23057, #1821, #1851, .T. ) ;
#18876 = CARTESIAN_POINT ( 'NONE',  ( -1.726321361862525858E-17, 3.783416666742532186, -0.2819296736111110979 ) ) ;
#18877 = CONICAL_SURFACE ( 'NONE', #7949, 1.243000000000000105, 0.2617993877991500740 ) ;
#18878 = DIRECTION ( 'NONE',  ( 0.000000000000000000, 0.000000000000000000, -1.000000000000000000 ) ) ;
#18879 = CARTESIAN_POINT ( 'NONE',  ( -0.2977100099089716734, 3.659999999999999698, 0.09499999999999995948 ) ) ;
#18880 = ORIENTED_EDGE ( 'NONE', *, *, #2767, .F. ) ;
#18881 = CARTESIAN_POINT ( 'NONE',  ( -0.1292346314604032043, 4.540361111111110404, -0.3120000000000024420 ) ) ;
#18882 = ORIENTED_EDGE ( 'NONE', *, *, #12864, .T. ) ;
#18883 = ADVANCED_FACE ( 'NONE', ( #17218 ), #5192, .T. ) ;
#18884 = CARTESIAN_POINT ( 'NONE',  ( -0.1733018972839396876, 4.121925556977420690, 0.2594426199919281917 ) ) ;
#18885 = CARTESIAN_POINT ( 'NONE',  ( -0.3155070326520293400, -0.1306872919485614626, -0.09743055555555497904 ) ) ;
#18886 = AXIS2_PLACEMENT_3D ( 'NONE', #703, #10106, #17411 ) ;
#18887 = ADVANCED_FACE ( 'NONE', ( #4283 ), #13695, .T. ) ;
#18888 = FACE_OUTER_BOUND ( 'NONE', #15286, .T. ) ;
#18889 = CARTESIAN_POINT ( 'NONE',  ( 0.2288853704217172214, 5.153467588116631859, -0.1971701303957707208 ) ) ;
#18890 = ORIENTED_EDGE ( 'NONE', *, *, #5096, .T. ) ;
#18891 = CARTESIAN_POINT ( 'NONE',  ( -0.3613381517857144343, 0.4080357141881717498, 0.1174058825155740171 ) ) ;
#18892 = CARTESIAN_POINT ( 'NONE',  ( -0.1167790944451424368, 0.5736111110352444253, 0.2819296736111110424 ) ) ;
#18893 = CARTESIAN_POINT ( 'NONE',  ( 0.2764156081756483641, 0.1144950937579610056, -0.09569444444444405451 ) ) ;
#18894 = CARTESIAN_POINT ( 'NONE',  ( 0.3129372601465110204, 0.4335988933679512103, -1.132625307779410395 ) ) ;
#18895 = DIRECTION ( 'NONE',  ( -0.000000000000000000, -1.000000000000000000, -0.000000000000000000 ) ) ;
#18896 = CARTESIAN_POINT ( 'NONE',  ( -0.2764156081756484196, -0.1144950937579609362, 0.2654166666666699093 ) ) ;
#18897 = VERTEX_POINT ( 'NONE', #10269 ) ;
#18898 = CARTESIAN_POINT ( 'NONE',  ( -0.3078090614149728288, 5.104275867521749888, -0.04150825043530404629 ) ) ;
#18899 = CARTESIAN_POINT ( 'NONE',  ( 0.4449999999999991740, 2.689999999999999947, 0.000000000000000000 ) ) ;
#18900 = LOCAL_TIME ( 21, 9, 13.00000000000000000, #20682 ) ;
#18901 = CARTESIAN_POINT ( 'NONE',  ( 0.3119999999999999996, 0.3513888888888885287, 0.000000000000000000 ) ) ;
#18902 = CARTESIAN_POINT ( 'NONE',  ( 0.2206173157302028787, 5.182722222222221120, 0.2206173157302027954 ) ) ;
#18903 = CARTESIAN_POINT ( 'NONE',  ( -0.2819296736111110979, 4.200083333409199149, 0.000000000000000000 ) ) ;
#18904 = CARTESIAN_POINT ( 'NONE',  ( -0.5116234456863258950, 1.999640111863030256, -2.727383698113316157 ) ) ;
#18905 = CYLINDRICAL_SURFACE ( 'NONE', #11047, 0.3125000000000000000 ) ;
#18906 = ORIENTED_EDGE ( 'NONE', *, *, #22273, .T. ) ;
#18907 = ADVANCED_FACE ( 'NONE', ( #15508 ), #19519, .T. ) ;
#18908 = CARTESIAN_POINT ( 'NONE',  ( 0.2819296736111110424, 4.884111111186975940, -0.1167790944451423396 ) ) ;
#18909 = AXIS2_PLACEMENT_3D ( 'NONE', #12395, #3223, #19812 ) ;
#18910 = EDGE_CURVE ( 'NONE', #21079, #24062, #11864, .T. ) ;
#18911 = CARTESIAN_POINT ( 'NONE',  ( 2.326421213736078119E-17, 0.3687499999024574371, -0.3799334167787516980 ) ) ;
#18912 = CARTESIAN_POINT ( 'NONE',  ( -0.2262210652167811753, 5.149889715124365885, -0.2008809606663144176 ) ) ;
#18913 = DIRECTION ( 'NONE',  ( 1.000000000000000000, 0.000000000000000000, 0.000000000000000000 ) ) ;
#18914 = CARTESIAN_POINT ( 'NONE',  ( -0.4687500000000003886, 0.2598076211353315124, 0.3779506566538943790 ) ) ;
#18915 = CYLINDRICAL_SURFACE ( 'NONE', #14995, 0.3119999999999999996 ) ;
#18916 = CARTESIAN_POINT ( 'NONE',  ( 0.1993543840281266633, 4.234805555631421470, -0.1993543840281266910 ) ) ;
#18917 = ITEM_DEFINED_TRANSFORMATION ( 'NONE', 'NONE', #4834,  #9127 ) ;
#18918 = ORIENTED_EDGE ( 'NONE', *, *, #12511, .T. ) ;
#18919 = DIRECTION ( 'NONE',  ( 0.000000000000000000, 0.000000000000000000, 1.000000000000000000 ) ) ;
#18920 = CARTESIAN_POINT ( 'NONE',  ( 0.2764156081756484196, -5.077672346800151106E-17, -0.04361111111111028865 ) ) ;
#18921 = CARTESIAN_POINT ( 'NONE',  ( 0.1993543840281266910, 0.6118055554796889561, -0.1993543840281266910 ) ) ;
#18922 = ORIENTED_EDGE ( 'NONE', *, *, #1692, .F. ) ;
#18923 = VECTOR ( 'NONE', #14661, 39.37007874015748854 ) ;
#18924 = CARTESIAN_POINT ( 'NONE',  ( 1.726321361862525858E-17, 0.4520833332574667462, -0.2819296736111110979 ) ) ;
#18925 = CARTESIAN_POINT ( 'NONE',  ( -1.910449006669871087E-17, 4.147999999999998799, -0.3119999999999999996 ) ) ;
#18926 = CARTESIAN_POINT ( 'NONE',  ( 9.101228903679513089E-16, 0.3732142855192008835, 0.4000000000000000222 ) ) ;
#18927 = AXIS2_PLACEMENT_3D ( 'NONE', #19945, #8716, #23581 ) ;
#18928 = CARTESIAN_POINT ( 'NONE',  ( 0.3236067977499789694, 0.2499999999999999167, 0.2351141009169893659 ) ) ;
#18929 = CARTESIAN_POINT ( 'NONE',  ( 0.2230971623002954429, 0.2230971623002953319, 0.09701388888889063422 ) ) ;
#18930 = CARTESIAN_POINT ( 'NONE',  ( -0.4254318749130439059, -0.3089257318245043349, 0.05347049744909274094 ) ) ;
#18931 = PLANE ( 'NONE',  #21421 ) ;
#18932 = CARTESIAN_POINT ( 'NONE',  ( -0.1993543840281266633, 0.2784722221463555858, -0.1993543840281266910 ) ) ;
#18933 = CARTESIAN_POINT ( 'NONE',  ( -0.2819296736111110979, 0.2333333332574667185, 0.1167790944451422425 ) ) ;
#18934 = EDGE_LOOP ( 'NONE', ( #22610, #2363, #17525, #23114 ) ) ;
#18935 = CARTESIAN_POINT ( 'NONE',  ( -0.1167790944451423535, 4.377166666742532186, 0.2819296736111110424 ) ) ;
#18936 = CARTESIAN_POINT ( 'NONE',  ( -0.3236067977499790249, 0.2910714283763437549, 0.2351141009169892271 ) ) ;
#18937 = CARTESIAN_POINT ( 'NONE',  ( -0.2819296736111110979, 4.922305555631420582, 0.000000000000000000 ) ) ;
#18938 = CARTESIAN_POINT ( 'NONE',  ( -1.726321361862525858E-17, 4.394527777853643791, -0.2819296736111110979 ) ) ;
#18939 = LINE ( 'NONE', #7595, #7518 ) ;
#18940 = APPROVAL_PERSON_ORGANIZATION ( #10047, #22227, #19418 ) ;
#18941 = ORIENTED_EDGE ( 'NONE', *, *, #18562, .T. ) ;
#18942 = LINE ( 'NONE', #9671, #3489 ) ;
#18943 = CARTESIAN_POINT ( 'NONE',  ( 0.2206173157302028787, 4.023000000151731648, 0.2206173157302027954 ) ) ;
#18944 = CARTESIAN_POINT ( 'NONE',  ( -0.3236067977499789694, 0.2767857140906294644, -0.2351141009169893104 ) ) ;
#18945 = CARTESIAN_POINT ( 'NONE',  ( -0.2742360776603882666, -0.1498359893665253684, -0.1016666666666679597 ) ) ;
#18946 = VERTEX_POINT ( 'NONE', #2348 ) ;
#18947 = DATE_AND_TIME ( #18700, #6443 ) ;
#18948 = CARTESIAN_POINT ( 'NONE',  ( -0.07866760015732025824, 0.03242967361111055713, 0.2712073892435483691 ) ) ;
#18949 = DIRECTION ( 'NONE',  ( -0.8660254037844526964, 0.000000000000000000, -0.4999999999999756306 ) ) ;
#18950 = ORIENTED_EDGE ( 'NONE', *, *, #479, .T. ) ;
#18951 = CARTESIAN_POINT ( 'NONE',  ( 0.3119999999999999996, 0.4034722220704893281, -0.1292346314604056468 ) ) ;
#18952 = ORIENTED_EDGE ( 'NONE', *, *, #7562, .F. ) ;
#18953 = CARTESIAN_POINT ( 'NONE',  ( -1.903245722532910002E-17, 5.100068075568266579, -0.3108236144263021861 ) ) ;
#18954 = DIRECTION ( 'NONE',  ( -0.000000000000000000, -1.000000000000000000, -0.000000000000000000 ) ) ;
#18955 = CARTESIAN_POINT ( 'NONE',  ( 0.005222582290261976699, 4.765907289028824323, -0.3119625414449602729 ) ) ;
#18956 = CARTESIAN_POINT ( 'NONE',  ( 0.3613381517857143232, 0.06160714275960043479, 0.1174058825155742114 ) ) ;
#18957 = CARTESIAN_POINT ( 'NONE',  ( 0.2782785630874277660, 5.176493536591711297, 0.09777844860489284806 ) ) ;
#18958 = ORIENTED_EDGE ( 'NONE', *, *, #17974, .F. ) ;
#18959 = CARTESIAN_POINT ( 'NONE',  ( 0.1116596296178199027, 0.4258928570453147100, 0.3436530038418508792 ) ) ;
#18960 = DIRECTION ( 'NONE',  ( 0.000000000000000000, 1.000000000000000000, 0.000000000000000000 ) ) ;
#18961 = CARTESIAN_POINT ( 'NONE',  ( -0.2300903070655175853, 4.675406423759836727, 0.2107194894688067810 ) ) ;
#18962 = CARTESIAN_POINT ( 'NONE',  ( 0.2819296736111110979, 4.102861111186976828, -3.452642723725051716E-17 ) ) ;
#18963 =( BOUNDED_SURFACE ( )  B_SPLINE_SURFACE ( 3, 2, ( 
 ( #21716, #12461, #15985 ),
 ( #19764, #3060, #10625 ),
 ( #16108, #19882, #5364 ),
 ( #24012, #3900, #11224 ),
 ( #7676, #12829, #15126 ),
 ( #5730, #3656, #3417 ),
 ( #7201, #7322, #241 ),
 ( #16472, #7440, #20484 ),
 ( #11102, #24125, #9391 ),
 ( #20248, #114, #22552 ),
 ( #12711, #5604, #9268 ),
 ( #16708, #11345, #20365 ) ),
 .UNSPECIFIED., .F., .F., .T. ) 
 B_SPLINE_SURFACE_WITH_KNOTS ( ( 4, 2, 2, 2, 2, 4 ),
 ( 3, 3 ),
 ( 0.04583429251981868680, 0.04917046297897018775, 0.05083854820854594170, 0.05250663343812168871, 0.05584280389727318966, 0.05917897435642469062 ),
 ( 0.000000000000000000, 1.000000000000000000 ),
 .UNSPECIFIED. ) 
 GEOMETRIC_REPRESENTATION_ITEM ( )  RATIONAL_B_SPLINE_SURFACE ( (
 ( 1.000000000000000000, 0.8464669816041905381, 1.000000000000000000),
 ( 1.000000000000000000, 0.8516145702047686061, 1.000000000000000000),
 ( 1.000000000000000000, 0.8565400046562395842, 1.000000000000000000),
 ( 1.000000000000000000, 0.8619820649909384347, 1.000000000000000000),
 ( 1.000000000000000000, 0.8634666681419451706, 1.000000000000000000),
 ( 1.000000000000000000, 0.8654947235244276893, 1.000000000000000000),
 ( 1.000000000000000000, 0.8660222433461404190, 1.000000000000000000),
 ( 1.000000000000000000, 0.8660316815622557396, 1.000000000000000000),
 ( 1.000000000000000000, 0.8638737604836346229, 1.000000000000000000),
 ( 1.000000000000000000, 0.8566366026603471351, 1.000000000000000000),
 ( 1.000000000000000000, 0.8516183347815020621, 1.000000000000000000),
 ( 1.000000000000000000, 0.8464669816041905381, 1.000000000000000000) ) ) 
 REPRESENTATION_ITEM ( '' )  SURFACE ( )  );
#18964 =( BOUNDED_CURVE ( )  B_SPLINE_CURVE ( 2, ( #16241, #23176, #6486, #1604, #18305, #3426, #16361, #23772, #3665 ),
 .UNSPECIFIED., .F., .T. ) 
 B_SPLINE_CURVE_WITH_KNOTS ( ( 3, 2, 2, 2, 3 ),
 ( 0.3660714285714285476, 0.3705357142857143016, 0.3750000000000000000, 0.3794642857142856429, 0.3839285714285713969 ),
 .UNSPECIFIED. ) 
 CURVE ( )  GEOMETRIC_REPRESENTATION_ITEM ( )  RATIONAL_B_SPLINE_CURVE ( ( 1.000000000000000000, 0.9238795325112867385, 1.000000000000000000, 0.9238795325112867385, 1.000000000000000000, 0.9238795325112867385, 1.000000000000000000, 0.9238795325112877377, 0.9999999999999990008 ) ) 
 REPRESENTATION_ITEM ( '' )  );
#18965 = CARTESIAN_POINT ( 'NONE',  ( -0.3832388449590500290, -0.3084783300535373640, 0.4166279060364119768 ) ) ;
#18966 = CARTESIAN_POINT ( 'NONE',  ( 1.243238971816016674E-16, 0.8949999999999999067, -1.015181661097394050 ) ) ;
#18967 = CARTESIAN_POINT ( 'NONE',  ( 1.910449006669871087E-17, 0.5874999999999996891, -0.3119999999999999996 ) ) ;
#18968 = CARTESIAN_POINT ( 'NONE',  ( 0.2206173157302028787, 4.689666666818398610, 0.2206173157302027954 ) ) ;
#18969 = CARTESIAN_POINT ( 'NONE',  ( 0.2819296736111110979, 4.950083333409199149, -3.452642723725051716E-17 ) ) ;
#18970 = ORIENTED_EDGE ( 'NONE', *, *, #5119, .T. ) ;
#18971 = CARTESIAN_POINT ( 'NONE',  ( 0.1167790944451424368, 4.370222222298088433, 0.2819296736111110424 ) ) ;
#18972 = B_SPLINE_CURVE_WITH_KNOTS ( 'NONE', 3,
 ( #7116, #20156, #24041, #9421, #3812, #5761, #1738, #14917, #18325, #14802, #145, #9298, #23794, #21978, #9177, #16738, #18804, #16621 ),
 .UNSPECIFIED., .F., .F.,
 ( 4, 2, 2, 2, 2, 2, 2, 2, 4 ),
 ( 0.000000000000000000, 0.001843124596548149008, 0.003686249193096298015, 0.005529373789644447673, 0.007372498386192604704, 0.009215622982740761734, 0.01105874757928891963, 0.01290187217583707580, 0.01474499677238523196 ),
 .UNSPECIFIED. ) ;
#18973 = ORIENTED_EDGE ( 'NONE', *, *, #14453, .T. ) ;
#18974 = VECTOR ( 'NONE', #5817, 39.37007874015748854 ) ;
#18975 = ORIENTED_EDGE ( 'NONE', *, *, #21038, .T. ) ;
#18976 = APPROVAL_ROLE ( '' ) ;
#18977 = DIRECTION ( 'NONE',  ( 0.000000000000000000, -0.000000000000000000, -1.000000000000000000 ) ) ;
#18978 = CARTESIAN_POINT ( 'NONE',  ( 1.509989503348686489E-16, 0.000000000000000000, -1.223000000000000309 ) ) ;
#18979 = CARTESIAN_POINT ( 'NONE',  ( -0.1167790944451423119, 3.967444444520310309, -0.2819296736111110979 ) ) ;
#18980 = LINE ( 'NONE', #13382, #15032 ) ;
#18981 = CARTESIAN_POINT ( 'NONE',  ( 0.006528205157002813994, -0.5487477722931476398, 0.04212966708837326962 ) ) ;
#18982 = LINE ( 'NONE', #15447, #20765 ) ;
#18983 = ORIENTED_EDGE ( 'NONE', *, *, #20260, .F. ) ;
#18984 = CARTESIAN_POINT ( 'NONE',  ( 0.1144950937579609085, -0.2764156081756484751, 0.2168055555555584990 ) ) ;
#18985 = CARTESIAN_POINT ( 'NONE',  ( -0.1167790944451424506, 0.5319444443685777957, 0.2819296736111110424 ) ) ;
#18986 = CARTESIAN_POINT ( 'NONE',  ( 0.000000000000000000, 0.2764156081756484196, 0.4702777777777826795 ) ) ;
#18987 = EDGE_LOOP ( 'NONE', ( #5945, #20508, #19203, #9808 ) ) ;
#18988 = CARTESIAN_POINT ( 'NONE',  ( 0.2819296736111110979, 4.946611111186976828, 0.1167790944451422425 ) ) ;
#18989 = CARTESIAN_POINT ( 'NONE',  ( -0.2206173157302027676, 3.946611111111110404, 0.2206173157302028787 ) ) ;
#18990 = EDGE_CURVE ( 'NONE', #10051, #16767, #20987, .T. ) ;
#18991 = CARTESIAN_POINT ( 'NONE',  ( 0.2819296736111110979, 4.766055555631421470, 0.1167790944451422425 ) ) ;
#18992 = CARTESIAN_POINT ( 'NONE',  ( -0.0003173656412832901504, 4.154953562412278423, -0.3119998790825884716 ) ) ;
#18993 = CARTESIAN_POINT ( 'NONE',  ( 0.2613201277241708476, 4.868437831976468289, -0.1709465549858873445 ) ) ;
#18994 = CARTESIAN_POINT ( 'NONE',  ( -0.09343526663134765764, 1.673690498276180818E-18, 0.3656947149432163147 ) ) ;
#18995 = LINE ( 'NONE', #5702, #6118 ) ;
#18996 = CARTESIAN_POINT ( 'NONE',  ( -0.3119999999999999996, 4.491749999999999687, -0.1292346314604056468 ) ) ;
#18997 = VECTOR ( 'NONE', #22996, 39.37007874015748854 ) ;
#18998 = CARTESIAN_POINT ( 'NONE',  ( -0.1993543840281266910, 3.734805555631421026, -0.1993543840281266910 ) ) ;
#18999 = CARTESIAN_POINT ( 'NONE',  ( 0.000000000000000000, 1.869379215919938807E-19, -0.01219352927422984872 ) ) ;
#19000 = ORIENTED_EDGE ( 'NONE', *, *, #12786, .T. ) ;
#19001 = CARTESIAN_POINT ( 'NONE',  ( 0.4687500000000002776, -0.2598076211353317344, 0.3779506566538943235 ) ) ;
#19002 = ORIENTED_EDGE ( 'NONE', *, *, #7661, .T. ) ;
#19003 = CARTESIAN_POINT ( 'NONE',  ( 0.1857256452555779147, 4.704968275741245876, -0.2517511420527552835 ) ) ;
#19004 = CARTESIAN_POINT ( 'NONE',  ( 0.06044521969078997525, 4.653203224452946429, -0.3063190883922444208 ) ) ;
#19005 = EDGE_CURVE ( 'NONE', #19709, #23209, #19232, .T. ) ;
#19006 = ADVANCED_FACE ( 'NONE', ( #17694 ), #22934, .T. ) ;
#19007 = CARTESIAN_POINT ( 'NONE',  ( -0.1306872919485614903, 0.3155070326520293400, -0.1668749999999999123 ) ) ;
#19008 = EDGE_CURVE ( 'NONE', #18846, #14964, #13404, .T. ) ;
#19009 = EDGE_CURVE ( 'NONE', #17212, #20917, #11061, .T. ) ;
#19010 = CARTESIAN_POINT ( 'NONE',  ( -0.05085398167855915974, 3.934169838589318235, -0.3079969485113711603 ) ) ;
#19011 = VERTEX_POINT ( 'NONE', #986 ) ;
#19012 = CARTESIAN_POINT ( 'NONE',  ( -0.1116596296178199582, 0.01517857133102903239, -0.3436530038418508792 ) ) ;
#19013 = CARTESIAN_POINT ( 'NONE',  ( -0.1167790944451422702, 0.5527777777019111660, -0.2819296736111110424 ) ) ;
#19014 = CARTESIAN_POINT ( 'NONE',  ( 2.824051777240061223E-14, 3.849388889040854522, 0.3119999999999999996 ) ) ;
#19015 = CARTESIAN_POINT ( 'NONE',  ( 0.3150097106828184113, 0.4536608415932815164, -1.126457079336245393 ) ) ;
#19016 = CARTESIAN_POINT ( 'NONE',  ( 2.369221741255291391, 0.000000000000000000, -1.763529041877836434 ) ) ;
#19017 = CARTESIAN_POINT ( 'NONE',  ( -0.1144950937579609918, -0.2764156081756484196, 0.1612500000000023914 ) ) ;
#19018 = ADVANCED_FACE ( 'NONE', ( #23161 ), #15629, .T. ) ;
#19019 = CARTESIAN_POINT ( 'NONE',  ( -0.1504314248901025552, 4.622694688059741708, 0.2733394608957197547 ) ) ;
#19020 = CARTESIAN_POINT ( 'NONE',  ( 0.3949999999999999623, 2.665000000000000036, -0.04999999999999915623 ) ) ;
#19021 = CARTESIAN_POINT ( 'NONE',  ( 4.312521114635084752E-13, 5.190332509204934830, -0.2890970118899086061 ) ) ;
#19022 = CARTESIAN_POINT ( 'NONE',  ( -0.3119999999999999996, 0.1569444444444440812, -3.820898013339742174E-17 ) ) ;
#19023 = CARTESIAN_POINT ( 'NONE',  ( 0.2206173157302027954, 5.141055555555555046, -0.2206173157302028232 ) ) ;
#19024 = CARTESIAN_POINT ( 'NONE',  ( -1.726321361862525858E-17, 4.241750000075866112, -0.2819296736111110979 ) ) ;
#19025 = CARTESIAN_POINT ( 'NONE',  ( -0.4453125000000000000, -5.968957943988233420E-17, 0.4425000000000000044 ) ) ;
#19026 = CARTESIAN_POINT ( 'NONE',  ( 0.000000000000000000, 0.1199999999999999956, 0.000000000000000000 ) ) ;
#19027 = CARTESIAN_POINT ( 'NONE',  ( 0.1236067977499789028, 0.3767857140906293867, 0.3804226065180614791 ) ) ;
#19028 = ORIENTED_EDGE ( 'NONE', *, *, #6476, .T. ) ;
#19029 = EDGE_LOOP ( 'NONE', ( #23487, #17174, #3578, #5612, #8186 ) ) ;
#19030 = CARTESIAN_POINT ( 'NONE',  ( 0.3119999999999999996, 0.3548611111111107386, -0.1292346314604056468 ) ) ;
#19031 = CARTESIAN_POINT ( 'NONE',  ( 0.2819296736111110424, 4.661888888964754507, -0.1167790944451423396 ) ) ;
#19032 = CARTESIAN_POINT ( 'NONE',  ( 0.3124999999999999445, 0.1294417382415923023, -0.01236111111110986711 ) ) ;
#19033 = DIRECTION ( 'NONE',  ( 0.000000000000000000, 0.000000000000000000, 1.000000000000000000 ) ) ;
#19034 = CARTESIAN_POINT ( 'NONE',  ( -3.385114897866767815E-17, -0.2764156081756484196, -0.1199999999999997735 ) ) ;
#19035 = CARTESIAN_POINT ( 'NONE',  ( -0.1167790944451423535, 4.210500000075866112, 0.2819296736111110979 ) ) ;
#19036 = DATE_AND_TIME ( #7816, #11566 ) ;
#19037 = CARTESIAN_POINT ( 'NONE',  ( -0.02453107547806535407, 4.044502971429987603, -0.3110395951528659442 ) ) ;
#19038 = CARTESIAN_POINT ( 'NONE',  ( 0.000000000000000000, 0.4987679491924311148, 0.000000000000000000 ) ) ;
#19039 = DIRECTION ( 'NONE',  ( -1.000000000000000000, 0.000000000000000000, 0.000000000000000000 ) ) ;
#19040 = AXIS2_PLACEMENT_3D ( 'NONE', #19211, #683, #2635 ) ;
#19041 = CARTESIAN_POINT ( 'NONE',  ( 0.1993543840281266910, 0.5562499999241333759, -0.1993543840281266910 ) ) ;
#19042 = LINE ( 'NONE', #380, #12763 ) ;
#19043 = CARTESIAN_POINT ( 'NONE',  ( -0.3236067977499790249, 0.3624999998049152072, 0.2351141009169892271 ) ) ;
#19044 = CARTESIAN_POINT ( 'NONE',  ( -0.3999999999999999667, 0.2892857142857141461, -0.1299678784931626030 ) ) ;
#19045 = CARTESIAN_POINT ( 'NONE',  ( -0.2230971623002953874, 0.2230971623002954152, 0.1109027777777796125 ) ) ;
#19046 = CARTESIAN_POINT ( 'NONE',  ( 0.000000000000000000, 5.384999999999999787, 0.000000000000000000 ) ) ;
#19047 = CARTESIAN_POINT ( 'NONE',  ( -8.183246661411124563E-08, 3.960496777434589610, 0.3119999999999772400 ) ) ;
#19048 = CARTESIAN_POINT ( 'NONE',  ( 0.1993543840281266355, 0.5840277777019111660, 0.1993543840281267465 ) ) ;
#19049 = CARTESIAN_POINT ( 'NONE',  ( 0.2819296736111110424, 0.1499999999241333482, -0.1167790944451423119 ) ) ;
#19050 = ORIENTED_EDGE ( 'NONE', *, *, #14108, .T. ) ;
#19051 = CARTESIAN_POINT ( 'NONE',  ( 0.1993543840281267465, 4.387583333409199149, 0.1993543840281266633 ) ) ;
#19052 = CARTESIAN_POINT ( 'NONE',  ( -0.3236067977499790249, 0.3624999998049152072, 0.2351141009169892271 ) ) ;
#19053 = CARTESIAN_POINT ( 'NONE',  ( -0.1167790944451423535, 4.821611111186976828, 0.2819296736111110424 ) ) ;
#19054 = CARTESIAN_POINT ( 'NONE',  ( 0.1993543840281266633, 4.332027777853642903, -0.1993543840281266910 ) ) ;
#19055 = CARTESIAN_POINT ( 'NONE',  ( 0.2206173157302027954, 4.529944444444443441, -0.2206173157302028232 ) ) ;
#19056 = CARTESIAN_POINT ( 'NONE',  ( 0.3119999999999999996, 3.918833333485065129, -3.820898013339742174E-17 ) ) ;
#19057 = CARTESIAN_POINT ( 'NONE',  ( -0.2472135954999579444, 0.2732142855192008501, -0.3402603233408160732 ) ) ;
#19058 =( LENGTH_UNIT ( ) NAMED_UNIT ( * ) SI_UNIT ( $, .METRE. ) );
#19059 = ORIENTED_EDGE ( 'NONE', *, *, #6472, .F. ) ;
#19060 = APPROVAL_ROLE ( '' ) ;
#19061 = CARTESIAN_POINT ( 'NONE',  ( 0.3999999999999999667, 0.3249999999999997891, 0.1299678784931626307 ) ) ;
#19062 = DIRECTION ( 'NONE',  ( -0.000000000000000000, -1.000000000000000000, -0.000000000000000000 ) ) ;
#19063 = CARTESIAN_POINT ( 'NONE',  ( -0.2491081030224410742, 4.996314154494937654, -0.1922342116985285287 ) ) ;
#19064 = ORIENTED_EDGE ( 'NONE', *, *, #6672, .T. ) ;
#19065 = CARTESIAN_POINT ( 'NONE',  ( -0.1167790944451422702, 0.1222222221463555858, -0.2819296736111110424 ) ) ;
#19066 = ORIENTED_EDGE ( 'NONE', *, *, #6236, .T. ) ;
#19067 = CARTESIAN_POINT ( 'NONE',  ( 1.750236327630675475E-17, 0.2749999999999999112, -0.3999999999999999667 ) ) ;
#19068 = DIRECTION ( 'NONE',  ( 0.000000000000000000, 0.000000000000000000, -1.000000000000000000 ) ) ;
#19069 = CARTESIAN_POINT ( 'NONE',  ( -0.4749999999999999778, 3.575000000000000622, 2.908536147974962357E-17 ) ) ;
#19070 = CARTESIAN_POINT ( 'NONE',  ( -0.2923287055106771337, 0.1080357141881718719, 0.2123892367102619971 ) ) ;
#19071 = CARTESIAN_POINT ( 'NONE',  ( 0.2842222223090039024, 5.180769402414656000, -0.07294254692603430179 ) ) ;
#19072 = ORIENTED_EDGE ( 'NONE', *, *, #14994, .F. ) ;
#19073 = LINE ( 'NONE', #9817, #9244 ) ;
#19074 = DIRECTION ( 'NONE',  ( -0.000000000000000000, -0.000000000000000000, -1.000000000000000000 ) ) ;
#19075 = CARTESIAN_POINT ( 'NONE',  ( -0.2764156081756484196, 0.1144950937579609918, 0.4181944444444490872 ) ) ;
#19076 = CARTESIAN_POINT ( 'NONE',  ( 0.2819296736111110979, 3.936194444520309865, -3.452642723725051716E-17 ) ) ;
#19077 = CARTESIAN_POINT ( 'NONE',  ( -0.1943163256447902609, -0.4290772944462951655, 0.4279515871991128040 ) ) ;
#19078 = CARTESIAN_POINT ( 'NONE',  ( 0.1533040153457264076, 5.122559226553594414, 0.2679359661953843452 ) ) ;
#19079 = CARTESIAN_POINT ( 'NONE',  ( -0.1781879481744626514, 5.169505967695794624, -0.2374271584184740325 ) ) ;
#19080 = CARTESIAN_POINT ( 'NONE',  ( -0.3119999999999998885, 4.783416666818398610, 0.1292346314604058410 ) ) ;
#19081 = CARTESIAN_POINT ( 'NONE',  ( 0.1167790944451422702, 5.016055555631420582, -0.2819296736111110979 ) ) ;
#19082 = EDGE_LOOP ( 'NONE', ( #16075, #8905, #22468, #7898 ) ) ;
#19083 = CARTESIAN_POINT ( 'NONE',  ( -0.1167790944451423535, 4.196611111186976828, 0.2819296736111110424 ) ) ;
#19084 = ORIENTED_EDGE ( 'NONE', *, *, #4798, .T. ) ;
#19085 = CARTESIAN_POINT ( 'NONE',  ( -0.3613381517857143232, 0.02946428561674330898, -4.425116109941954795E-17 ) ) ;
#19086 = ORIENTED_EDGE ( 'NONE', *, *, #11214, .F. ) ;
#19087 = CIRCLE ( 'NONE', #5065, 0.7500000000000001110 ) ;
#19088 = ORIENTED_EDGE ( 'NONE', *, *, #24094, .T. ) ;
#19089 = APPROVAL_ROLE ( '' ) ;
#19090 = DIRECTION ( 'NONE',  ( -0.000000000000000000, 1.000000000000000000, -0.000000000000000000 ) ) ;
#19091 = DIRECTION ( 'NONE',  ( 0.000000000000000000, -1.000000000000000000, 0.000000000000000000 ) ) ;
#19092 = CARTESIAN_POINT ( 'NONE',  ( -0.1993543840281266910, 3.970916666742532186, -0.1993543840281266910 ) ) ;
#19093 = CYLINDRICAL_SURFACE ( 'NONE', #10750, 0.3119999999999999996 ) ;
#19094 = DIRECTION ( 'NONE',  ( 0.8660254037844382635, 0.000000000000000000, -0.5000000000000004441 ) ) ;
#19095 =( BOUNDED_CURVE ( )  B_SPLINE_CURVE ( 2, ( #4026, #4267, #15248, #20729, #4383, #11716, #20612, #2563, #18781 ),
 .UNSPECIFIED., .F., .F. ) 
 B_SPLINE_CURVE_WITH_KNOTS ( ( 3, 2, 2, 2, 3 ),
 ( 0.4479166666666667407, 0.4583333333333334259, 0.4687500000000001110, 0.4791666666666667962, 0.4895833333333334814 ),
 .UNSPECIFIED. ) 
 CURVE ( )  GEOMETRIC_REPRESENTATION_ITEM ( )  RATIONAL_B_SPLINE_CURVE ( ( 0.9999999999999995559, 0.9238795325112871826, 1.000000000000000000, 0.9238795325112867385, 1.000000000000000000, 0.9238795325112867385, 1.000000000000000000, 0.9238795325112859613, 1.000000000000000888 ) ) 
 REPRESENTATION_ITEM ( '' )  );
#19096 = CARTESIAN_POINT ( 'NONE',  ( 0.2721215285213450241, -0.3841564396211945565, 0.07944889038202707088 ) ) ;
#19097 = CARTESIAN_POINT ( 'NONE',  ( 0.2764156081756484196, -5.077672346800151106E-17, 0.2272222222222252119 ) ) ;
#19098 = CARTESIAN_POINT ( 'NONE',  ( -0.2819296736111111534, 0.5249999999241332649, 0.1167790944451422563 ) ) ;
#19099 = CARTESIAN_POINT ( 'NONE',  ( 0.1144950937579609085, -0.2764156081756484751, 0.3904166666666708529 ) ) ;
#19100 = ORIENTED_EDGE ( 'NONE', *, *, #16313, .T. ) ;
#19101 = CARTESIAN_POINT ( 'NONE',  ( -0.2819296736111110424, 4.696611111186977716, -0.1167790944451423119 ) ) ;
#19102 = CARTESIAN_POINT ( 'NONE',  ( -0.06335377612981457629, 0.4428123468925277417, 0.3999999999999999667 ) ) ;
#19103 = CARTESIAN_POINT ( 'NONE',  ( -0.2819296736111110424, 4.745222222298088433, 0.1167790944451424923 ) ) ;
#19104 = CARTESIAN_POINT ( 'NONE',  ( 0.000000000000000000, 5.384999999999999787, -0.3119999999999999996 ) ) ;
#19105 = TOROIDAL_SURFACE ( 'NONE', #17, 0.2510000000000000009, 0.0009999999999999859262 ) ;
#19106 = CARTESIAN_POINT ( 'NONE',  ( -0.3125000000000000000, 1.913510623667739771E-17, 0.3383333333333369830 ) ) ;
#19107 = LINE ( 'NONE', #4107, #14913 ) ;
#19108 = CARTESIAN_POINT ( 'NONE',  ( -5.731347020009612645E-17, 0.2194444442927115380, 0.3119999999999999996 ) ) ;
#19109 = CARTESIAN_POINT ( 'NONE',  ( 0.1292346314604056190, 4.366749999999998799, -0.3119999999999999996 ) ) ;
#19110 = AXIS2_PLACEMENT_3D ( 'NONE', #2932, #2462, #6589 ) ;
#19111 = CARTESIAN_POINT ( 'NONE',  ( -0.2472135954999579999, 0.3035714285714284366, 0.3402603233408160732 ) ) ;
#19112 = FACE_OUTER_BOUND ( 'NONE', #15047, .T. ) ;
#19113 = VERTEX_POINT ( 'NONE', #23047 ) ;
#19114 = DIRECTION ( 'NONE',  ( 0.8660254037844438146, 0.000000000000000000, 0.4999999999999910627 ) ) ;
#19115 = ORIENTED_EDGE ( 'NONE', *, *, #1482, .T. ) ;
#19116 = CARTESIAN_POINT ( 'NONE',  ( 0.2596173626562791603, 4.701861296690032610, -0.1735006093349389100 ) ) ;
#19117 = EDGE_CURVE ( 'NONE', #3680, #15369, #23004, .T. ) ;
#19118 = CARTESIAN_POINT ( 'NONE',  ( 0.4788584550258475625, -0.2689697488930788416, 0.04193801346286649828 ) ) ;
#19119 = CARTESIAN_POINT ( 'NONE',  ( 0.000000000000000000, 0.2764156081756484196, 0.4077777777777822354 ) ) ;
#19120 = CIRCLE ( 'NONE', #3156, 1.048989065017511546 ) ;
#19121 = CARTESIAN_POINT ( 'NONE',  ( -0.1005310964907748239, 3.935617334977024928, -0.2960650091076030277 ) ) ;
#19122 = EDGE_LOOP ( 'NONE', ( #4735, #6112, #6072, #22677 ) ) ;
#19123 = CARTESIAN_POINT ( 'NONE',  ( 0.2233192592356399164, -0.01696428581182810730, 0.3073725909049500604 ) ) ;
#19124 = CARTESIAN_POINT ( 'NONE',  ( 0.1993543840281266910, 0.4868055554796889561, -0.1993543840281266910 ) ) ;
#19125 = LINE ( 'NONE', #9747, #10171 ) ;
#19126 = CARTESIAN_POINT ( 'NONE',  ( 0.1015149863201169345, 0.7712941925382441610, -1.079846890036118667 ) ) ;
#19127 = CARTESIAN_POINT ( 'NONE',  ( -0.2464202454315806146, -0.1619151084082731396, -0.08350906156777793132 ) ) ;
#19128 = CARTESIAN_POINT ( 'NONE',  ( 0.000000000000000000, 0.2764156081756484196, 0.1925000000000026690 ) ) ;
#19129 = CARTESIAN_POINT ( 'NONE',  ( -0.2637094125609521500, 5.109987496479720726, 0.1629003720249567189 ) ) ;
#19130 = CARTESIAN_POINT ( 'NONE',  ( 0.01848103877824584448, 0.5441716683897389606, 0.04413116910601658227 ) ) ;
#19131 = CARTESIAN_POINT ( 'NONE',  ( -0.009437680304838758777, 4.101846522467919178E-18, -0.3821420945942993752 ) ) ;
#19132 = CARTESIAN_POINT ( 'NONE',  ( -0.3119999999999999996, 0.2124999999999996336, -3.820898013339742174E-17 ) ) ;
#19133 = CARTESIAN_POINT ( 'NONE',  ( -0.1292346314604057023, 5.172305555555555046, 0.3119999999999998885 ) ) ;
#19134 = CARTESIAN_POINT ( 'NONE',  ( 0.1167790944451424368, 4.106333333409199149, 0.2819296736111110424 ) ) ;
#19135 = CARTESIAN_POINT ( 'NONE',  ( -0.2206173157302028232, 3.821611111111110404, -0.2206173157302028232 ) ) ;
#19136 = DIRECTION ( 'NONE',  ( 0.000000000000000000, 0.000000000000000000, -1.000000000000000000 ) ) ;
#19137 = DIRECTION ( 'NONE',  ( 0.000000000000000000, 0.000000000000000000, 1.000000000000000000 ) ) ;
#19138 = ORIENTED_EDGE ( 'NONE', *, *, #3399, .T. ) ;
#19139 = EDGE_CURVE ( 'NONE', #21365, #22483, #7280, .T. ) ;
#19140 = CARTESIAN_POINT ( 'NONE',  ( 0.3062750282812972125, 0.05890668782135718290, 0.4221389973272440810 ) ) ;
#19141 = CARTESIAN_POINT ( 'NONE',  ( 0.1993543840281266633, 4.665361111186976828, -0.1993543840281266910 ) ) ;
#19142 = CARTESIAN_POINT ( 'NONE',  ( 0.3613381517857143232, 0.3473214284738860291, 0.1174058825155741975 ) ) ;
#19143 = CARTESIAN_POINT ( 'NONE',  ( -0.04381235360356670883, 4.514848399031694548, 0.3091263664638504438 ) ) ;
#19144 = EDGE_CURVE ( 'NONE', #19164, #4009, #15721, .T. ) ;
#19145 = SHAPE_DEFINITION_REPRESENTATION ( #6796, #4490 ) ;
#19146 = DIRECTION ( 'NONE',  ( 0.000000000000000000, 0.000000000000000000, 1.000000000000000000 ) ) ;
#19147 = CARTESIAN_POINT ( 'NONE',  ( 0.1144950937579609085, -0.2764156081756484751, -0.1165277777777775636 ) ) ;
#19148 = CARTESIAN_POINT ( 'NONE',  ( -0.1167790944451423119, 4.300777777853643791, -0.2819296736111110979 ) ) ;
#19149 = APPROVAL_ROLE ( '' ) ;
#19150 = CARTESIAN_POINT ( 'NONE',  ( 0.3119999999999999996, 4.304249999999999687, -0.1292346314604056745 ) ) ;
#19151 = CARTESIAN_POINT ( 'NONE',  ( 0.009375000000000072511, -0.5358532185916218271, 0.4425000000000000044 ) ) ;
#19152 = DIRECTION ( 'NONE',  ( -0.000000000000000000, -1.000000000000000000, -0.000000000000000000 ) ) ;
#19153 = ORIENTED_EDGE ( 'NONE', *, *, #11438, .T. ) ;
#19154 = CARTESIAN_POINT ( 'NONE',  ( -0.1167790944451424368, 0.4763888888130222710, 0.2819296736111110424 ) ) ;
#19155 = DIRECTION ( 'NONE',  ( 0.000000000000000000, 1.000000000000000000, 0.000000000000000000 ) ) ;
#19156 = DIRECTION ( 'NONE',  ( 0.000000000000000000, 0.000000000000000000, -1.000000000000000000 ) ) ;
#19157 = CARTESIAN_POINT ( 'NONE',  ( 3.820898013339742174E-17, 5.384999999999999787, 0.3119999999999999996 ) ) ;
#19158 = CARTESIAN_POINT ( 'NONE',  ( -0.3155070326520292845, 1.931923388228935888E-17, 0.2289583333333361503 ) ) ;
#19159 = DIRECTION ( 'NONE',  ( 1.224646799147354193E-16, 0.000000000000000000, -1.000000000000000000 ) ) ;
#19160 = EDGE_CURVE ( 'NONE', #17972, #8592, #14369, .T. ) ;
#19161 = FACE_OUTER_BOUND ( 'NONE', #5951, .T. ) ;
#19162 = CARTESIAN_POINT ( 'NONE',  ( 0.1993543840281266355, 0.4729166665908000611, 0.1993543840281267465 ) ) ;
#19163 = CARTESIAN_POINT ( 'NONE',  ( -5.178964085587577574E-17, 0.2437499999241333204, 0.2819296736111110979 ) ) ;
#19164 = VERTEX_POINT ( 'NONE', #4998 ) ;
#19165 = CARTESIAN_POINT ( 'NONE',  ( 0.1993543840281267465, 4.220916666742532186, 0.1993543840281266633 ) ) ;
#19166 = CARTESIAN_POINT ( 'NONE',  ( 0.3236067977499789694, 0.3124999998049152183, 0.2351141009169893659 ) ) ;
#19167 = CARTESIAN_POINT ( 'NONE',  ( 0.2819296736111110979, 4.838972222298088433, -3.452642723725051716E-17 ) ) ;
#19168 = CARTESIAN_POINT ( 'NONE',  ( -0.2819296736111110424, 4.245222222298087544, 0.1167790944451424923 ) ) ;
#19169 = EDGE_CURVE ( 'NONE', #22410, #20541, #2500, .T. ) ;
#19170 = FACE_OUTER_BOUND ( 'NONE', #16169, .T. ) ;
#19171 = EDGE_CURVE ( 'NONE', #2257, #20185, #23762, .T. ) ;
#19172 = ORIENTED_EDGE ( 'NONE', *, *, #4852, .F. ) ;
#19173 = CARTESIAN_POINT ( 'NONE',  ( 0.1292346314604080892, 4.533416666666665762, -0.3119999999999975016 ) ) ;
#19174 = CARTESIAN_POINT ( 'NONE',  ( 0.1292346314604056190, 3.762583333485065573, -0.3119999999999999996 ) ) ;
#19175 = CARTESIAN_POINT ( 'NONE',  ( 2.557132486540519611, 0.000000000000000000, -2.541000000000000369 ) ) ;
#19176 = ORIENTED_EDGE ( 'NONE', *, *, #5129, .F. ) ;
#19177 = CALENDAR_DATE ( 2026, 7, 10 ) ;
#19178 = CONICAL_SURFACE ( 'NONE', #872, 0.4062499999999995004, 0.7853981633974482790 ) ;
#19179 = CARTESIAN_POINT ( 'NONE',  ( 0.000000000000000000, 0.4987679491924311148, 0.000000000000000000 ) ) ;
#19180 = CARTESIAN_POINT ( 'NONE',  ( -0.2499270801673589282, 5.007890031258386720, 0.1869623468028804858 ) ) ;
#19181 = ORIENTED_EDGE ( 'NONE', *, *, #14139, .F. ) ;
#19182 = CARTESIAN_POINT ( 'NONE',  ( 1.726321361862525858E-17, 0.1743055554796889284, -0.2819296736111110979 ) ) ;
#19183 = CARTESIAN_POINT ( 'NONE',  ( 0.01790655108702505355, 4.265571681436381546, -0.3115083198477991422 ) ) ;
#19184 = CARTESIAN_POINT ( 'NONE',  ( 0.006542161132012710989, 0.5374887588746247724, 0.3892820121258430688 ) ) ;
#19185 = DIRECTION ( 'NONE',  ( 0.000000000000000000, 1.000000000000000000, 0.000000000000000000 ) ) ;
#19186 = CARTESIAN_POINT ( 'NONE',  ( 0.3613381517857143232, -0.002678571526113826800, -0.1174058825155740587 ) ) ;
#19187 = CARTESIAN_POINT ( 'NONE',  ( 0.2635902294012452129, 5.175512519792486721, 0.1331235142709102925 ) ) ;
#19188 = ORIENTED_EDGE ( 'NONE', *, *, #23255, .T. ) ;
#19189 = DIRECTION ( 'NONE',  ( 0.000000000000000000, 0.000000000000000000, 1.000000000000000000 ) ) ;
#19190 = CARTESIAN_POINT ( 'NONE',  ( -0.07935600121137664775, 4.680387721508536103, 0.3045026414546517235 ) ) ;
#19191 = CARTESIAN_POINT ( 'NONE',  ( -1.726321361862525858E-17, 3.894527777853643347, -0.2819296736111110979 ) ) ;
#19192 = CARTESIAN_POINT ( 'NONE',  ( -0.06362248101067675965, 0.03486971683296733598, 0.2776287047131382191 ) ) ;
#19193 = CARTESIAN_POINT ( 'NONE',  ( -0.2135870376730847342, 5.171211814165030063, -0.2053538857893718594 ) ) ;
#19194 = CARTESIAN_POINT ( 'NONE',  ( 0.1292346314604056190, 4.429250000151731648, -0.3119999999999999996 ) ) ;
#19195 = VECTOR ( 'NONE', #423, 39.37007874015748143 ) ;
#19196 = CARTESIAN_POINT ( 'NONE',  ( -0.2819296736111110979, 4.918833333409199149, -0.1167790944451422980 ) ) ;
#19197 = EDGE_LOOP ( 'NONE', ( #2624, #22381, #9919, #18950 ) ) ;
#19198 = CARTESIAN_POINT ( 'NONE',  ( 0.1167790944451424368, 4.314666666742532186, 0.2819296736111110424 ) ) ;
#19199 = ORIENTED_EDGE ( 'NONE', *, *, #24008, .F. ) ;
#19200 = EDGE_CURVE ( 'NONE', #5943, #15066, #10696, .T. ) ;
#19201 = ADVANCED_FACE ( 'NONE', ( #3291 ), #4881, .T. ) ;
#19202 = ORIENTED_EDGE ( 'NONE', *, *, #22981, .T. ) ;
#19203 = ORIENTED_EDGE ( 'NONE', *, *, #16780, .F. ) ;
#19204 = DATE_TIME_ROLE ( 'classification_date' ) ;
#19205 = ORIENTED_EDGE ( 'NONE', *, *, #14841, .F. ) ;
#19206 = CARTESIAN_POINT ( 'NONE',  ( 0.4788479876972290827, 0.2689986204937583336, 0.04193567535760913539 ) ) ;
#19207 = CARTESIAN_POINT ( 'NONE',  ( 0.4749999999999999778, 3.700000000000000622, 0.09499999999999998723 ) ) ;
#19208 = CARTESIAN_POINT ( 'NONE',  ( 0.3119999999999999996, 0.06666666651493373397, 0.000000000000000000 ) ) ;
#19209 = VECTOR ( 'NONE', #5966, 39.37007874015747433 ) ;
#19210 = CARTESIAN_POINT ( 'NONE',  ( 0.07064684460510516073, 4.406932727029926333, 0.3038970684541104084 ) ) ;
#19211 = CARTESIAN_POINT ( 'NONE',  ( -0.01874999999999989869, -0.5520911949125800744, 0.06112444011295371793 ) ) ;
#19212 = CARTESIAN_POINT ( 'NONE',  ( 0.2773501192371399804, -0.3936383244008247462, 0.07440066028685882182 ) ) ;
#19213 = CARTESIAN_POINT ( 'NONE',  ( -0.2764156081756484196, 1.692557448933383907E-17, 0.3105555555555591929 ) ) ;
#19214 = CARTESIAN_POINT ( 'NONE',  ( -0.1993543840281267465, 0.4173611110352444253, 0.1993543840281266633 ) ) ;
#19215 = CARTESIAN_POINT ( 'NONE',  ( -0.1954553509668046918, -0.1954553509668046640, -0.07138888888888827999 ) ) ;
#19216 = VERTEX_POINT ( 'NONE', #1349 ) ;
#19217 = CARTESIAN_POINT ( 'NONE',  ( 0.1993543840281267465, 4.665361111186976828, 0.1993543840281266633 ) ) ;
#19218 = CARTESIAN_POINT ( 'NONE',  ( 0.003294150194310348223, -0.5383638965977115554, 0.05893128447555213284 ) ) ;
#19219 = CARTESIAN_POINT ( 'NONE',  ( 0.2819296736111110424, 4.661888888964754507, -0.1167790944451423396 ) ) ;
#19220 = CARTESIAN_POINT ( 'NONE',  ( 0.2206173157302028232, 0.2958333331816003775, -0.2206173157302028232 ) ) ;
#19221 = CARTESIAN_POINT ( 'NONE',  ( -0.1294417382415922746, -0.3125000000000000000, 0.3487500000000036682 ) ) ;
#19222 = DIRECTION ( 'NONE',  ( -0.000000000000000000, -1.000000000000000000, -0.000000000000000000 ) ) ;
#19223 = CARTESIAN_POINT ( 'NONE',  ( 0.000000000000000000, 5.384999999999999787, 0.000000000000000000 ) ) ;
#19224 = CARTESIAN_POINT ( 'NONE',  ( 0.3119999999999999996, 4.189666666666665762, -3.820898013339742174E-17 ) ) ;
#19225 = DIRECTION ( 'NONE',  ( 0.000000000000000000, 0.000000000000000000, 1.000000000000000000 ) ) ;
#19226 = CARTESIAN_POINT ( 'NONE',  ( -0.2206173157302028232, 5.161888889040620931, -0.2206173157302028232 ) ) ;
#19227 = CARTESIAN_POINT ( 'NONE',  ( -0.1292346314604105872, 3.984805555555555046, -0.3119999999999950591 ) ) ;
#19228 = CC_DESIGN_PERSON_AND_ORGANIZATION_ASSIGNMENT ( #6884, #4928, ( #11526 ) ) ;
#19229 = ORIENTED_EDGE ( 'NONE', *, *, #24084, .T. ) ;
#19230 = DIRECTION ( 'NONE',  ( 0.000000000000000000, -1.000000000000000000, 0.000000000000000000 ) ) ;
#19231 = ORIENTED_EDGE ( 'NONE', *, *, #8863, .T. ) ;
#19232 = CIRCLE ( 'NONE', #7926, 0.3125000000000001665 ) ;
#19233 = CARTESIAN_POINT ( 'NONE',  ( 0.1902844741700089604, 4.688494737640487742, 0.2506308059723901249 ) ) ;
#19234 = DESIGN_CONTEXT ( 'detailed design', #23822, 'design' ) ;
#19235 = DIRECTION ( 'NONE',  ( 0.000000000000000000, 0.000000000000000000, -1.000000000000000000 ) ) ;
#19236 = CARTESIAN_POINT ( 'NONE',  ( -0.2764156081756484196, 1.692557448933383907E-17, 0.4216666666666711860 ) ) ;
#19237 = CARTESIAN_POINT ( 'NONE',  ( 1.750236327630675537E-16, 0.02499999999999997710, 0.3999999999999999667 ) ) ;
#19238 = VERTEX_POINT ( 'NONE', #23881 ) ;
#19239 = EDGE_CURVE ( 'NONE', #14583, #20092, #13207, .T. ) ;
#19240 = CARTESIAN_POINT ( 'NONE',  ( -0.2923287055106771337, 0.03660714275960045422, 0.2123892367102619971 ) ) ;
#19241 = CARTESIAN_POINT ( 'NONE',  ( 0.2819296736111110979, 0.5354166665908000056, 0.000000000000000000 ) ) ;
#19242 = PLANE ( 'NONE',  #14450 ) ;
#19243 = DIRECTION ( 'NONE',  ( -0.000000000000000000, -1.000000000000000000, -0.000000000000000000 ) ) ;
#19244 = CARTESIAN_POINT ( 'NONE',  ( -0.05416907386917569484, -0.2729753724328098374, -0.06690562264081034716 ) ) ;
#19245 = CARTESIAN_POINT ( 'NONE',  ( 0.1954553509668046640, -0.1954553509668047195, 0.2827777777777811807 ) ) ;
#19246 = ORIENTED_EDGE ( 'NONE', *, *, #18731, .T. ) ;
#19247 = CARTESIAN_POINT ( 'NONE',  ( -0.09000656359012888796, 4.624632385561261216, 0.3024265629511137532 ) ) ;
#19248 = FACE_OUTER_BOUND ( 'NONE', #13587, .T. ) ;
#19249 = FACE_BOUND ( 'NONE', #10924, .T. ) ;
#19250 = CARTESIAN_POINT ( 'NONE',  ( 0.2206173157302027676, 0.2333333333333330040, 0.2206173157302028787 ) ) ;
#19251 = CARTESIAN_POINT ( 'NONE',  ( 5.731347020009612645E-17, 4.842444444444443441, 0.3119999999999999996 ) ) ;
#19252 = PRODUCT_DEFINITION ( 'UNKNOWN', '', #17744, #19234 ) ;
#19253 = CARTESIAN_POINT ( 'NONE',  ( 0.1993543840281267465, 3.887583333409199149, 0.1993543840281266633 ) ) ;
#19254 = CYLINDRICAL_SURFACE ( 'NONE', #309, 0.4000000000000000222 ) ;
#19255 = CARTESIAN_POINT ( 'NONE',  ( -0.4228029066818159709, 0.2971605053783716865, 0.3901413544830086844 ) ) ;
#19256 = LINE ( 'NONE', #23380, #11834 ) ;
#19257 = VERTEX_POINT ( 'NONE', #16470 ) ;
#19258 = VERTEX_POINT ( 'NONE', #7200 ) ;
#19259 = CARTESIAN_POINT ( 'NONE',  ( 0.4620259694561523744, 0.2880908832651560281, 0.04413116910601654758 ) ) ;
#19260 = CARTESIAN_POINT ( 'NONE',  ( 0.1993543840281266633, 4.776472222298087544, -0.1993543840281266910 ) ) ;
#19261 = CARTESIAN_POINT ( 'NONE',  ( 0.4620259694561523744, -0.2880908832651558615, 0.04413116910601658921 ) ) ;
#19262 = CARTESIAN_POINT ( 'NONE',  ( 0.2530612899223194101, -0.3951608735071495682, 0.4181572966874575470 ) ) ;
#19263 = AXIS2_PLACEMENT_3D ( 'NONE', #14755, #1691, #11085 ) ;
#19264 = PERSON_AND_ORGANIZATION_ROLE ( 'design_owner' ) ;
#19265 = CARTESIAN_POINT ( 'NONE',  ( 3.073863465859856523E-17, 5.500232050807569273, 0.2510000000000000009 ) ) ;
#19266 = CARTESIAN_POINT ( 'NONE',  ( 0.2764156081756483641, -0.1144950937579611167, -0.1095833333333330328 ) ) ;
#19267 = CARTESIAN_POINT ( 'NONE',  ( -0.1167790944451423535, 4.377166666742532186, 0.2819296736111110979 ) ) ;
#19268 = CARTESIAN_POINT ( 'NONE',  ( -0.2437001351828723128, 4.051746529912200856, -0.1987809944906386850 ) ) ;
#19269 = CARTESIAN_POINT ( 'NONE',  ( -0.1954553509668046918, -0.1954553509668046640, 0.04666666666666818841 ) ) ;
#19270 = APPROVAL_PERSON_ORGANIZATION ( #5654, #13438, #10914 ) ;
#19271 = CARTESIAN_POINT ( 'NONE',  ( 3.820898013339742174E-17, 5.384999999999999787, 0.3119999999999999996 ) ) ;
#19272 = ORIENTED_EDGE ( 'NONE', *, *, #12302, .F. ) ;
#19273 = CARTESIAN_POINT ( 'NONE',  ( -5.178964085587577574E-17, 0.4798611110352444253, 0.2819296736111110979 ) ) ;
#19274 = CARTESIAN_POINT ( 'NONE',  ( 0.3119999999999999996, 4.134111111111110404, -3.820898013339742174E-17 ) ) ;
#19275 = CARTESIAN_POINT ( 'NONE',  ( -0.5116234456863466562, 0.9548081934128057613, 2.725603391761944660 ) ) ;
#19276 = CARTESIAN_POINT ( 'NONE',  ( -0.3125000000000002776, 0.1294417382415919970, 0.001527777777778780745 ) ) ;
#19277 = CARTESIAN_POINT ( 'NONE',  ( 0.3155070326520292845, -5.795770164686806123E-17, 0.09006944444444611730 ) ) ;
#19278 = EDGE_LOOP ( 'NONE', ( #10220, #16399, #2392, #6365 ) ) ;
#19279 = CARTESIAN_POINT ( 'NONE',  ( 0.000000000000000000, 5.501232050807569607, -0.2510000000000000009 ) ) ;
#19280 = CARTESIAN_POINT ( 'NONE',  ( 0.3950000000000000178, 0.04999999999999921868, -0.04999999999999915623 ) ) ;
#19281 = CARTESIAN_POINT ( 'NONE',  ( -0.2819296736111111534, 0.3999999999241333204, 0.1167790944451422563 ) ) ;
#19282 = CARTESIAN_POINT ( 'NONE',  ( -0.1993543840281267465, 0.2368055554796889561, 0.1993543840281266633 ) ) ;
#19283 = ORIENTED_EDGE ( 'NONE', *, *, #23423, .T. ) ;
#19284 = CARTESIAN_POINT ( 'NONE',  ( -0.1167790944451423257, 4.134111111186977716, -0.2819296736111110424 ) ) ;
#19285 = CARTESIAN_POINT ( 'NONE',  ( 0.3999999999999999667, 0.3946428569477722359, -0.1299678784931625475 ) ) ;
#19286 = CIRCLE ( 'NONE', #7212, 0.01875000000000000971 ) ;
#19287 = EDGE_CURVE ( 'NONE', #5871, #15814, #22067, .T. ) ;
#19288 = CARTESIAN_POINT ( 'NONE',  ( 0.1993543840281267465, 4.776472222298088433, 0.1993543840281266633 ) ) ;
#19289 = CARTESIAN_POINT ( 'NONE',  ( 0.3999999999999999667, 0.1732142855192008724, 0.1299678784931626307 ) ) ;
#19290 = ORIENTED_EDGE ( 'NONE', *, *, #11008, .F. ) ;
#19291 = CARTESIAN_POINT ( 'NONE',  ( 0.3125000000000009437, -0.1294417382415913309, 0.2515277777777808477 ) ) ;
#19292 = CARTESIAN_POINT ( 'NONE',  ( 5.731347020009612645E-17, 3.960500000151731648, 0.3119999999999999996 ) ) ;
#19293 = LOCAL_TIME ( 21, 9, 13.00000000000000000, #2152 ) ;
#19294 = CARTESIAN_POINT ( 'NONE',  ( 0.1309139991617564724, -0.2436136748879755842, 0.3880822748423154445 ) ) ;
#19295 =( NAMED_UNIT ( * ) PLANE_ANGLE_UNIT ( ) SI_UNIT ( $, .RADIAN. ) );
#19296 = ORIENTED_EDGE ( 'NONE', *, *, #2030, .T. ) ;
#19297 = PERSON_AND_ORGANIZATION ( #15518, #2538 ) ;
#19298 = AXIS2_PLACEMENT_3D ( 'NONE', #10568, #21523, #4813 ) ;
#19299 = LINE ( 'NONE', #11514, #3135 ) ;
#19300 = EDGE_CURVE ( 'NONE', #7081, #5165, #2936, .T. ) ;
#19301 = EDGE_CURVE ( 'NONE', #18008, #7579, #12582, .T. ) ;
#19302 = CARTESIAN_POINT ( 'NONE',  ( -0.2648550963346621434, 5.007173855133585150, 0.1658120503390664024 ) ) ;
#19303 = ORIENTED_EDGE ( 'NONE', *, *, #8564, .T. ) ;
#19304 = CARTESIAN_POINT ( 'NONE',  ( 0.2819296736111110424, 0.1083333332574667046, -0.1167790944451423119 ) ) ;
#19305 = EDGE_CURVE ( 'NONE', #9833, #4879, #8541, .T. ) ;
#19306 = VERTEX_POINT ( 'NONE', #6712 ) ;
#19307 = CARTESIAN_POINT ( 'NONE',  ( 0.1308302654899865247, 4.262330775219983714, -0.2839942560154425921 ) ) ;
#19308 = CARTESIAN_POINT ( 'NONE',  ( 0.1366666852802012888, 0.4623613298294839691, 0.4215068951509038930 ) ) ;
#19309 = DIRECTION ( 'NONE',  ( 0.000000000000000000, 0.000000000000000000, -1.000000000000000000 ) ) ;
#19310 = CARTESIAN_POINT ( 'NONE',  ( 0.3613381517857143232, 0.3544642856167432576, -0.1174058825155740587 ) ) ;
#19311 = CARTESIAN_POINT ( 'NONE',  ( 0.2549033356607801060, 5.182729380544451203, -0.1438613240065718113 ) ) ;
#19312 =( BOUNDED_CURVE ( )  B_SPLINE_CURVE ( 2, ( #10134, #23264, #15731, #12211, #6575, #2567, #13681, #17437, #15374 ),
 .UNSPECIFIED., .F., .T. ) 
 B_SPLINE_CURVE_WITH_KNOTS ( ( 3, 2, 2, 2, 3 ),
 ( 0.7410714285714286031, 0.7455357142857143016, 0.7500000000000000000, 0.7544642857142855874, 0.7589285714285712858 ),
 .UNSPECIFIED. ) 
 CURVE ( )  GEOMETRIC_REPRESENTATION_ITEM ( )  RATIONAL_B_SPLINE_CURVE ( ( 1.000000000000000000, 0.9238795325112867385, 1.000000000000000000, 0.9238795325112867385, 1.000000000000000000, 0.9238795325112867385, 1.000000000000000000, 0.9238795325112886259, 0.9999999999999981126 ) ) 
 REPRESENTATION_ITEM ( '' )  );
#19313 = ORIENTED_EDGE ( 'NONE', *, *, #11828, .T. ) ;
#19314 = LOCAL_TIME ( 21, 9, 13.00000000000000000, #11756 ) ;
#19315 = CARTESIAN_POINT ( 'NONE',  ( -0.3613381517857143788, 0.4080357141881718053, 0.1174058825155740310 ) ) ;
#19316 = B_SPLINE_CURVE_WITH_KNOTS ( 'NONE', 3,
 ( #18786, #19388, #19745, #10377, #11848, #2798, #15849, #23035, #23148, #19504, #4741, #12092 ),
 .UNSPECIFIED., .F., .F.,
 ( 4, 2, 2, 2, 2, 4 ),
 ( 0.000000000000000000, 0.003384026746073586205, 0.006768053492147172411, 0.008460066865183961393, 0.01015208023822075124, 0.01353610698429432921 ),
 .UNSPECIFIED. ) ;
#19317 = FACE_OUTER_BOUND ( 'NONE', #7251, .T. ) ;
#19318 = EDGE_CURVE ( 'NONE', #7560, #14944, #14157, .T. ) ;
#19319 = CARTESIAN_POINT ( 'NONE',  ( 5.178964085587577574E-17, 3.922305555631421026, 0.2819296736111110979 ) ) ;
#19320 = CARTESIAN_POINT ( 'NONE',  ( -0.1948874010148252123, -0.4287475839276986278, 0.4171140917644005630 ) ) ;
#19321 = CARTESIAN_POINT ( 'NONE',  ( -0.2000768274382927203, 5.170541012004494341, -0.2188383321351891897 ) ) ;
#19322 = CIRCLE ( 'NONE', #22433, 0.01874999999999997155 ) ;
#19323 = LINE ( 'NONE', #2621, #13232 ) ;
#19324 = CARTESIAN_POINT ( 'NONE',  ( -0.1292346314604056745, 4.602861111262843252, -0.3119999999999999996 ) ) ;
#19325 = CARTESIAN_POINT ( 'NONE',  ( -1.726321361862525858E-17, 4.963972222298088433, -0.2819296736111110979 ) ) ;
#19326 = ORIENTED_EDGE ( 'NONE', *, *, #10045, .F. ) ;
#19327 = CARTESIAN_POINT ( 'NONE',  ( -0.2819296736111110424, 3.960500000075865668, -0.1167790944451423119 ) ) ;
#19328 = VERTEX_POINT ( 'NONE', #3059 ) ;
#19329 = ORIENTED_EDGE ( 'NONE', *, *, #566, .F. ) ;
#19330 = EDGE_LOOP ( 'NONE', ( #4665, #7752, #6131, #9780, #8352, #10233, #20798, #11769, #21522, #3664, #23339, #23862, #10505, #13485, #10552, #11597, #8504 ) ) ;
#19331 = PERSON_AND_ORGANIZATION ( #15518, #2538 ) ;
#19332 = ORIENTED_EDGE ( 'NONE', *, *, #23647, .F. ) ;
#19333 = DIRECTION ( 'NONE',  ( 0.000000000000000000, 0.000000000000000000, -1.000000000000000000 ) ) ;
#19334 = CARTESIAN_POINT ( 'NONE',  ( 0.3119999999999998885, 0.2923611111111107386, 0.1292346314604058410 ) ) ;
#19335 = CARTESIAN_POINT ( 'NONE',  ( 0.2206173157302027676, 0.1152777776260448528, 0.2206173157302028787 ) ) ;
#19336 = VECTOR ( 'NONE', #6738, 39.37007874015748854 ) ;
#19337 = CARTESIAN_POINT ( 'NONE',  ( 0.1998324900780631963, 5.137374311756707890, 0.2310110508733242141 ) ) ;
#19338 = CARTESIAN_POINT ( 'NONE',  ( -0.4687500000000003886, 0.08851153507826334255, 0.4142570404818415319 ) ) ;
#19339 = CARTESIAN_POINT ( 'NONE',  ( -0.4687500000000004441, -0.2174879564497122775, 0.3901672915530228214 ) ) ;
#19340 = FACE_OUTER_BOUND ( 'NONE', #1253, .T. ) ;
#19341 = CARTESIAN_POINT ( 'NONE',  ( -0.1144950937579609918, -0.2764156081756484196, 0.1543055555555579716 ) ) ;
#19342 = CARTESIAN_POINT ( 'NONE',  ( -0.1167790944451422702, 0.1083333332574667046, -0.2819296736111110979 ) ) ;
#19343 = CARTESIAN_POINT ( 'NONE',  ( 0.1144950937579611444, 0.2764156081756483641, 0.01541666666666797678 ) ) ;
#19344 = EDGE_CURVE ( 'NONE', #13713, #22476, #14565, .T. ) ;
#19345 = CARTESIAN_POINT ( 'NONE',  ( -1.726321361862525858E-17, 4.741750000075866112, -0.2819296736111110979 ) ) ;
#19346 = CARTESIAN_POINT ( 'NONE',  ( -0.1993543840281266355, 4.582027777853642903, 0.1993543840281267465 ) ) ;
#19347 = DIRECTION ( 'NONE',  ( -0.000000000000000000, -1.000000000000000000, -0.000000000000000000 ) ) ;
#19348 = CARTESIAN_POINT ( 'NONE',  ( 0.02327375635197577106, 4.850116391403974880, 0.3120000040497944993 ) ) ;
#19349 = CARTESIAN_POINT ( 'NONE',  ( 0.04612308010668176445, 4.715469205126319992E-18, 0.3680979378183042439 ) ) ;
#19350 = DIRECTION ( 'NONE',  ( 1.000000000000000000, 0.000000000000000000, 0.000000000000000000 ) ) ;
#19351 = CARTESIAN_POINT ( 'NONE',  ( 0.3119999999999999996, 4.356333333333332725, -3.820898013339742174E-17 ) ) ;
#19352 = CARTESIAN_POINT ( 'NONE',  ( 0.2206173157302028787, 5.134111111262843252, 0.2206173157302027954 ) ) ;
#19353 = CARTESIAN_POINT ( 'NONE',  ( 0.06225566914758315362, 4.962242484901489448, 0.3057257872088504635 ) ) ;
#19354 = EDGE_LOOP ( 'NONE', ( #9739, #8473, #12179, #17735 ) ) ;
#19355 = AXIS2_PLACEMENT_3D ( 'NONE', #6831, #6467, #21349 ) ;
#19356 = CARTESIAN_POINT ( 'NONE',  ( 0.1294417382415924134, 0.3124999999999999445, 0.2098611111111137462 ) ) ;
#19357 = EDGE_LOOP ( 'NONE', ( #15053, #10529, #4827, #311 ) ) ;
#19358 = CARTESIAN_POINT ( 'NONE',  ( 0.2823011957516836645, 4.700511095951428686, -0.1328541025166166123 ) ) ;
#19359 = CARTESIAN_POINT ( 'NONE',  ( 0.1903147850440313482, 4.133000686346171015, 0.2472334505447376096 ) ) ;
#19360 = CARTESIAN_POINT ( 'NONE',  ( -0.1306872919485615459, -0.3155070326520293400, 0.02062500000000154141 ) ) ;
#19361 = CARTESIAN_POINT ( 'NONE',  ( 0.2721904660997503944, 0.3841166384917397703, 0.07944544255957622370 ) ) ;
#19362 = CARTESIAN_POINT ( 'NONE',  ( -0.08089596400723292335, 3.935038355344236738, -0.3020212475751637982 ) ) ;
#19363 = CARTESIAN_POINT ( 'NONE',  ( -0.3613381517857144343, -0.03839285724039952913, 0.1174058825155740171 ) ) ;
#19364 = VECTOR ( 'NONE', #1019, 39.37007874015748854 ) ;
#19365 = LINE ( 'NONE', #10228, #16757 ) ;
#19366 = CARTESIAN_POINT ( 'NONE',  ( -0.2764156081756484196, 0.1144950937579609918, -0.1304166666666665420 ) ) ;
#19367 = CARTESIAN_POINT ( 'NONE',  ( 0.3613381517857143232, 0.01517857133102903412, -0.1174058825155740587 ) ) ;
#19368 = CARTESIAN_POINT ( 'NONE',  ( -0.3006586688675891850, -0.04349558104364664030, -0.09283059900161595712 ) ) ;
#19369 = CARTESIAN_POINT ( 'NONE',  ( 0.2764156081756483641, -0.1144950937579611167, 0.3418055555555594704 ) ) ;
#19370 = ORIENTED_EDGE ( 'NONE', *, *, #18421, .F. ) ;
#19371 = EDGE_CURVE ( 'NONE', #12633, #9048, #5842, .T. ) ;
#19372 = CARTESIAN_POINT ( 'NONE',  ( 1.679791495769851560E-14, 3.793833333485275183, 0.3119999999999999996 ) ) ;
#19373 = CARTESIAN_POINT ( 'NONE',  ( 0.3236067977499789694, 0.09821428551920090289, 0.2351141009169893659 ) ) ;
#19374 = CARTESIAN_POINT ( 'NONE',  ( -0.02524939306089188373, -3.088309080874367638E-17, -0.3822476892351002742 ) ) ;
#19375 = CARTESIAN_POINT ( 'NONE',  ( -5.731347020009612645E-17, 0.5597222222222218990, 0.3119999999999999996 ) ) ;
#19376 = CARTESIAN_POINT ( 'NONE',  ( 0.1292346314604058410, 4.901472222222222008, 0.3119999999999998885 ) ) ;
#19377 = CARTESIAN_POINT ( 'NONE',  ( 0.1167790944451424368, 4.050777777853643791, 0.2819296736111110424 ) ) ;
#19378 = DIRECTION ( 'NONE',  ( -0.000000000000000000, -1.000000000000000000, -0.000000000000000000 ) ) ;
#19379 = LINE ( 'NONE', #13902, #20675 ) ;
#19380 = CARTESIAN_POINT ( 'NONE',  ( 0.3719562388801891939, 2.800349848324033442, -1.181074844845517058 ) ) ;
#19381 = VERTEX_POINT ( 'NONE', #20720 ) ;
#19382 = ORIENTED_EDGE ( 'NONE', *, *, #19752, .T. ) ;
#19383 = DIRECTION ( 'NONE',  ( -0.000000000000000000, -1.000000000000000000, -0.000000000000000000 ) ) ;
#19384 = CARTESIAN_POINT ( 'NONE',  ( -0.1167790944451423535, 4.641055555631422358, 0.2819296736111110424 ) ) ;
#19385 = CARTESIAN_POINT ( 'NONE',  ( -0.2923287055106771337, 0.3223214284738861735, 0.2123892367102619971 ) ) ;
#19386 = CARTESIAN_POINT ( 'NONE',  ( 0.009375000000000065573, -0.5358532185916218271, 0.3779506566538943235 ) ) ;
#19387 = VECTOR ( 'NONE', #13074, 39.37007874015748143 ) ;
#19388 = CARTESIAN_POINT ( 'NONE',  ( 0.4209440094115191044, 0.2863418823927886825, 0.4064695056028758691 ) ) ;
#19389 = CARTESIAN_POINT ( 'NONE',  ( 0.1954553509668047195, 0.1954553509668046085, -0.04361111111111028865 ) ) ;
#19390 = CARTESIAN_POINT ( 'NONE',  ( 0.2819296736111110979, 4.398000000075866112, -0.1167790944451423396 ) ) ;
#19391 = APPROVAL ( #9044, 'UNSPECIFIED' ) ;
#19392 = CARTESIAN_POINT ( 'NONE',  ( -0.009374999999999905978, -0.5358532185916218271, 0.06112444011295371793 ) ) ;
#19393 = CARTESIAN_POINT ( 'NONE',  ( 0.000000000000000000, 0.2764156081756484196, 0.3036111111111146621 ) ) ;
#19394 = CARTESIAN_POINT ( 'NONE',  ( 0.3125000000000004996, -0.1294417382415918583, 0.3695833333333375936 ) ) ;
#19395 = ORIENTED_EDGE ( 'NONE', *, *, #20172, .T. ) ;
#19396 = CARTESIAN_POINT ( 'NONE',  ( -0.2819296736111110979, 0.5249999999241332649, 0.1167790944451422425 ) ) ;
#19397 = CARTESIAN_POINT ( 'NONE',  ( -0.2206173157302028787, 0.1083333333333329901, 0.2206173157302027954 ) ) ;
#19398 = CARTESIAN_POINT ( 'NONE',  ( 1.910449006669871087E-17, 0.2541666666666663188, -0.3119999999999999996 ) ) ;
#19399 = CARTESIAN_POINT ( 'NONE',  ( 0.2472135954999579166, 0.3892857142857142350, 0.3402603233408160732 ) ) ;
#19400 = CARTESIAN_POINT ( 'NONE',  ( 0.3155070326520292290, 0.1306872919485615736, 0.2602083333333364279 ) ) ;
#19401 = DIRECTION ( 'NONE',  ( 1.000000000000000000, 0.000000000000000000, -0.000000000000000000 ) ) ;
#19402 = CARTESIAN_POINT ( 'NONE',  ( 0.2209708691207961651, 0.2209708691207959985, 0.3730555555555594704 ) ) ;
#19403 = CARTESIAN_POINT ( 'NONE',  ( -0.2819296736111110979, 0.5631944443685777957, -3.452642723725051716E-17 ) ) ;
#19404 = CARTESIAN_POINT ( 'NONE',  ( 0.2819296736111110424, 0.4208333332574666352, 0.1167790944451424923 ) ) ;
#19405 = VERTEX_POINT ( 'NONE', #7796 ) ;
#19406 = CARTESIAN_POINT ( 'NONE',  ( -1.726321361862525858E-17, 4.019527777853643791, -0.2819296736111110979 ) ) ;
#19407 = TOROIDAL_SURFACE ( 'NONE', #22115, 0.6209078282299125284, 0.01874999999999999931 ) ;
#19408 = CARTESIAN_POINT ( 'NONE',  ( 2.575339694675500462E-17, 0.2660714283763437882, -0.4205848896953069405 ) ) ;
#19409 = CARTESIAN_POINT ( 'NONE',  ( 5.178964085587577574E-17, 4.602861111186976828, 0.2819296736111110979 ) ) ;
#19410 = ORIENTED_EDGE ( 'NONE', *, *, #13083, .T. ) ;
#19411 = CARTESIAN_POINT ( 'NONE',  ( 0.000000000000000000, 0.9040586665785882436, 0.000000000000000000 ) ) ;
#19412 = CARTESIAN_POINT ( 'NONE',  ( 0.2206173157302028787, 3.800777777929510215, 0.2206173157302027954 ) ) ;
#19413 = CARTESIAN_POINT ( 'NONE',  ( 0.000000000000000000, 5.580232050807569344, 0.000000000000000000 ) ) ;
#19414 = EDGE_CURVE ( 'NONE', #9355, #4761, #113, .T. ) ;
#19415 = LENGTH_MEASURE_WITH_UNIT ( LENGTH_MEASURE( 0.02539999999999999897 ), #8071 );
#19416 = ORIENTED_EDGE ( 'NONE', *, *, #24068, .T. ) ;
#19417 = VECTOR ( 'NONE', #23098, 39.37007874015748143 ) ;
#19418 = APPROVAL_ROLE ( '' ) ;
#19419 = EDGE_CURVE ( 'NONE', #6543, #23182, #7159, .T. ) ;
#19420 = CARTESIAN_POINT ( 'NONE',  ( 0.1841151976024382186, 0.2183016720772839037, 0.3966205073423086924 ) ) ;
#19421 = CARTESIAN_POINT ( 'NONE',  ( 0.9074166975080198982, 2.740000000000000213, -2.936000000000001720 ) ) ;
#19422 = VERTEX_POINT ( 'NONE', #18651 ) ;
#19423 = CARTESIAN_POINT ( 'NONE',  ( 0.2819296736111110979, 0.1604166665908000333, 0.000000000000000000 ) ) ;
#19424 = ORIENTED_EDGE ( 'NONE', *, *, #228, .T. ) ;
#19425 = CARTESIAN_POINT ( 'NONE',  ( 1.750236327630675537E-16, 0.02499999999999997710, 0.3999999999999999667 ) ) ;
#19426 = CARTESIAN_POINT ( 'NONE',  ( -0.3112102497767363363, 4.723343425208045510, -0.03524716832280518769 ) ) ;
#19427 = CARTESIAN_POINT ( 'NONE',  ( 1.750236327630675475E-17, 0.3374999998049151295, -0.3999999999999999667 ) ) ;
#19428 = CARTESIAN_POINT ( 'NONE',  ( 0.1116596296178199027, 0.1937499999024575870, 0.3436530038418508792 ) ) ;
#19429 = LINE ( 'NONE', #23195, #15913 ) ;
#19430 = CARTESIAN_POINT ( 'NONE',  ( -0.3613381517857143232, 0.4008928570453146878, -0.1174058825155741143 ) ) ;
#19431 = ORIENTED_EDGE ( 'NONE', *, *, #23851, .T. ) ;
#19432 = CARTESIAN_POINT ( 'NONE',  ( -0.4000000000000000222, 0.1446428569477723469, 0.1299678784931624920 ) ) ;
#19433 = CARTESIAN_POINT ( 'NONE',  ( 0.1167790944451424368, 3.759111111186976828, 0.2819296736111110424 ) ) ;
#19434 = DIRECTION ( 'NONE',  ( -0.000000000000000000, 0.9961946980917454342, -0.08715574274765824914 ) ) ;
#19435 = CARTESIAN_POINT ( 'NONE',  ( -0.2209942451922433382, 5.187717628303036399, 0.1882505735780611034 ) ) ;
#19436 = DIRECTION ( 'NONE',  ( -0.000000000000000000, -1.000000000000000000, -0.000000000000000000 ) ) ;
#19437 = CARTESIAN_POINT ( 'NONE',  ( -0.1292346314604057023, 4.623694444596176290, 0.3119999999999998885 ) ) ;
#19438 = CARTESIAN_POINT ( 'NONE',  ( -0.2819296736111110979, 4.755638888964754507, 0.000000000000000000 ) ) ;
#19439 = EDGE_CURVE ( 'NONE', #7539, #17359, #8312, .T. ) ;
#19440 = CARTESIAN_POINT ( 'NONE',  ( -0.1167790944451423257, 4.064666666742532186, -0.2819296736111110424 ) ) ;
#19441 = ADVANCED_FACE ( 'NONE', ( #3535 ), #9631, .T. ) ;
#19442 = CARTESIAN_POINT ( 'NONE',  ( 0.2923287055106771337, 0.2866071427596004195, -0.2123892367102620249 ) ) ;
#19443 = VERTEX_POINT ( 'NONE', #11343 ) ;
#19444 = ORIENTED_EDGE ( 'NONE', *, *, #7562, .T. ) ;
#19445 = SECURITY_CLASSIFICATION_LEVEL ( 'unclassified' ) ;
#19446 = EDGE_CURVE ( 'NONE', #16899, #13618, #17062, .T. ) ;
#19447 =( BOUNDED_CURVE ( )  B_SPLINE_CURVE ( 2, ( #19712, #8620, #3015, #10463, #16061, #23475, #6791, #14230, #22263 ),
 .UNSPECIFIED., .F., .T. ) 
 B_SPLINE_CURVE_WITH_KNOTS ( ( 3, 2, 2, 2, 3 ),
 ( 0.3229166666666666852, 0.3333333333333333703, 0.3437500000000000000, 0.3541666666666667407, 0.3645833333333334259 ),
 .UNSPECIFIED. ) 
 CURVE ( )  GEOMETRIC_REPRESENTATION_ITEM ( )  RATIONAL_B_SPLINE_CURVE ( ( 1.000000000000000444, 0.9238795325112862944, 1.000000000000000000, 0.9238795325112867385, 1.000000000000000000, 0.9238795325112867385, 1.000000000000000000, 0.9238795325112862944, 1.000000000000000444 ) ) 
 REPRESENTATION_ITEM ( '' )  );
#19448 = CYLINDRICAL_SURFACE ( 'NONE', #16953, 0.01874999999999997155 ) ;
#19449 = CARTESIAN_POINT ( 'NONE',  ( 0.2206173157302028232, 0.3027777777777774237, -0.2206173157302028232 ) ) ;
#19450 = CARTESIAN_POINT ( 'NONE',  ( 0.4592339806827420712, 0.08949080555460971198, 0.4305896728713884958 ) ) ;
#19451 = VECTOR ( 'NONE', #8884, 39.37007874015748143 ) ;
#19452 = CARTESIAN_POINT ( 'NONE',  ( 1.910449006669871087E-17, 0.5805555554038225319, -0.3119999999999999996 ) ) ;
#19453 = CARTESIAN_POINT ( 'NONE',  ( -0.4687500000000003331, 0.2208780317832466089, 0.4012013675560013315 ) ) ;
#19454 = CARTESIAN_POINT ( 'NONE',  ( 0.2209708691207961095, -0.2209708691207961651, -0.07833333333333258874 ) ) ;
#19455 = CARTESIAN_POINT ( 'NONE',  ( 7.478516849590708700E-17, -0.5289902422706634910, 0.3941886329748525153 ) ) ;
#19456 = CARTESIAN_POINT ( 'NONE',  ( -0.1167790944451424506, 0.07361111103524446697, 0.2819296736111110424 ) ) ;
#19457 = CARTESIAN_POINT ( 'NONE',  ( -0.1954553509668046640, 0.1954553509668046918, 0.02583333333333472440 ) ) ;
#19458 = ORIENTED_EDGE ( 'NONE', *, *, #2615, .F. ) ;
#19459 = DIRECTION ( 'NONE',  ( 0.000000000000000000, -0.9961946980917454342, 0.08715574274765833240 ) ) ;
#19460 = CARTESIAN_POINT ( 'NONE',  ( 0.1993543840281267465, 4.540361111186976828, 0.1993543840281266633 ) ) ;
#19461 = CARTESIAN_POINT ( 'NONE',  ( 0.1261236974911665865, 0.2628820852880351944, -0.08058443713070109760 ) ) ;
#19462 = CARTESIAN_POINT ( 'NONE',  ( -0.04114923329550543296, 0.1818063343982506408, -1.242004357290043881 ) ) ;
#19463 = DIRECTION ( 'NONE',  ( 0.8660254037844443697, 0.000000000000000000, 0.4999999999999901745 ) ) ;
#19464 = DIRECTION ( 'NONE',  ( 0.000000000000000000, 0.000000000000000000, -1.000000000000000000 ) ) ;
#19465 = CARTESIAN_POINT ( 'NONE',  ( -0.3119999999999999996, 4.217444444444443441, 0.000000000000000000 ) ) ;
#19466 = CARTESIAN_POINT ( 'NONE',  ( 0.1292346314604056190, 5.151472222373953969, -0.3119999999999999996 ) ) ;
#19467 = CARTESIAN_POINT ( 'NONE',  ( 0.1754988631321229564, 4.983003950203682031, -0.2618203274534778857 ) ) ;
#19468 = EDGE_LOOP ( 'NONE', ( #23611, #19002, #8195, #9265 ) ) ;
#19469 = CARTESIAN_POINT ( 'NONE',  ( 0.03717937511614839707, 4.572701828437388372, 0.3120000032059407902 ) ) ;
#19470 = B_SPLINE_CURVE_WITH_KNOTS ( 'NONE', 3,
 ( #5105, #11212, #8895, #23870, #1932, #16696, #18163, #9133, #5477, #5225, #5351, #16578, #11091, #18403, #18520, #23999, #1810, #12818, #19992, #7190 ),
 .UNSPECIFIED., .F., .F.,
 ( 4, 2, 2, 2, 2, 2, 2, 2, 2, 4 ),
 ( 0.5025725185951905871, 0.5048557457206661603, 0.5071389728461416224, 0.5094221999716171956, 0.5117054270970926577, 0.5139886542225682309, 0.5162718813480438040, 0.5185551084735192662, 0.5196967220362570528, 0.5208383355989948393 ),
 .UNSPECIFIED. ) ;
#19471 = ORIENTED_EDGE ( 'NONE', *, *, #7969, .T. ) ;
#19472 = CARTESIAN_POINT ( 'NONE',  ( 0.003051384878943240540, 4.710417945387369798, -0.3119872305879987651 ) ) ;
#19473 = UNCERTAINTY_MEASURE_WITH_UNIT (LENGTH_MEASURE( 1.000000000000000082E-05 ), #12478, 'distance_accuracy_value', 'NONE');
#19474 = EDGE_CURVE ( 'NONE', #21597, #2535, #10988, .T. ) ;
#19475 = CARTESIAN_POINT ( 'NONE',  ( 0.000000000000000000, 0.9300000000000000488, 1.015181661097394050 ) ) ;
#19476 = CARTESIAN_POINT ( 'NONE',  ( 0.000000000000000000, 0.3155070326520292845, -0.05923611111111021232 ) ) ;
#19477 = CARTESIAN_POINT ( 'NONE',  ( 0.1571283475654022266, 3.798372783338246794, 0.2726217976190928871 ) ) ;
#19478 = ORIENTED_EDGE ( 'NONE', *, *, #13462, .T. ) ;
#19479 = VECTOR ( 'NONE', #1678, 39.37007874015748143 ) ;
#19480 = CARTESIAN_POINT ( 'NONE',  ( -0.3613381517857143232, 0.3116071427596003862, -0.1174058825155741004 ) ) ;
#19481 = VECTOR ( 'NONE', #17095, 39.37007874015748143 ) ;
#19482 = CARTESIAN_POINT ( 'NONE',  ( 0.2819296736111110979, 0.1638888888130222432, -0.1167790944451422980 ) ) ;
#19483 = CARTESIAN_POINT ( 'NONE',  ( -0.1144950937579609918, -0.2764156081756484196, 0.05013888888889045381 ) ) ;
#19484 = CARTESIAN_POINT ( 'NONE',  ( 0.000000000000000000, 5.384999999999999787, 0.000000000000000000 ) ) ;
#19485 = CARTESIAN_POINT ( 'NONE',  ( -0.1954553509668046640, 0.1954553509668046918, 0.3105555555555591929 ) ) ;
#19486 = ORIENTED_EDGE ( 'NONE', *, *, #15132, .T. ) ;
#19487 = DIRECTION ( 'NONE',  ( 0.000000000000000000, 0.000000000000000000, -1.000000000000000000 ) ) ;
#19488 = CARTESIAN_POINT ( 'NONE',  ( -0.008647338669235882930, 4.293587880010775848, 0.3118972423166174179 ) ) ;
#19489 = CARTESIAN_POINT ( 'NONE',  ( -0.07178572706788863278, 2.632010880910626829E-18, -0.3787435909716683757 ) ) ;
#19490 = CARTESIAN_POINT ( 'NONE',  ( -0.3119999999999999996, 0.4347222222222218435, -3.820898013339742174E-17 ) ) ;
#19491 = CARTESIAN_POINT ( 'NONE',  ( -0.3119999999999999996, 5.047305555555555046, -0.1292346314604056468 ) ) ;
#19492 = CARTESIAN_POINT ( 'NONE',  ( -0.2819296736111110424, 4.085500000075865223, -0.1167790944451423119 ) ) ;
#19493 = CARTESIAN_POINT ( 'NONE',  ( -0.3119999999999999996, 0.5909722220704892726, -0.1292346314604056745 ) ) ;
#19494 = CARTESIAN_POINT ( 'NONE',  ( -0.3296559951169086844, 0.3509388998445532315, 0.4107594315541606700 ) ) ;
#19495 = DIRECTION ( 'NONE',  ( -0.000000000000000000, -0.000000000000000000, 1.000000000000000000 ) ) ;
#19496 = ORIENTED_EDGE ( 'NONE', *, *, #8284, .T. ) ;
#19497 = VERTEX_POINT ( 'NONE', #3779 ) ;
#19498 = LINE ( 'NONE', #2681, #24111 ) ;
#19499 = CARTESIAN_POINT ( 'NONE',  ( -0.1167790944451423257, 4.731333333409198261, -0.2819296736111110424 ) ) ;
#19500 = CARTESIAN_POINT ( 'NONE',  ( -0.02182715984130906631, 4.515461111269364558, 0.3112388426647295647 ) ) ;
#19501 = AXIS2_PLACEMENT_3D ( 'NONE', #17594, #16250, #23660 ) ;
#19502 = EDGE_CURVE ( 'NONE', #11153, #17792, #3265, .T. ) ;
#19503 = DIRECTION ( 'NONE',  ( 0.000000000000000000, 0.000000000000000000, 1.000000000000000000 ) ) ;
#19504 = CARTESIAN_POINT ( 'NONE',  ( 0.07572755880264359085, 0.4860218594902849798, 0.4166771511014252805 ) ) ;
#19505 = CARTESIAN_POINT ( 'NONE',  ( -0.2764156081756484196, -0.1144950937579609362, -0.01930555555555453148 ) ) ;
#19506 = LINE ( 'NONE', #972, #6876 ) ;
#19507 = CARTESIAN_POINT ( 'NONE',  ( -0.2819296736111110424, 4.036888888964755395, 0.1167790944451424923 ) ) ;
#19508 = DATE_TIME_ROLE ( 'classification_date' ) ;
#19509 = CARTESIAN_POINT ( 'NONE',  ( 0.4057955023597048516, 2.693521551442877193, -0.6418853869074238050 ) ) ;
#19510 = DIRECTION ( 'NONE',  ( 0.000000000000000000, 0.9659258262890680902, 0.2588190451025215721 ) ) ;
#19511 = CARTESIAN_POINT ( 'NONE',  ( -0.1954553509668046640, 0.1954553509668046918, 0.1438888888888912032 ) ) ;
#19512 = CARTESIAN_POINT ( 'NONE',  ( 0.3999999999999999667, 0.2607142857142855652, -0.1299678784931625197 ) ) ;
#19513 = CARTESIAN_POINT ( 'NONE',  ( -0.2819296736111110979, 0.01111111103524447911, 0.1167790944451422425 ) ) ;
#19514 = CARTESIAN_POINT ( 'NONE',  ( -0.2705345477997521120, 0.1189582700827291617, 0.4070486123150025004 ) ) ;
#19515 = CARTESIAN_POINT ( 'NONE',  ( -0.2206173157302027954, 0.4277777777777774237, -0.2206173157302028232 ) ) ;
#19516 = PLANE ( 'NONE',  #23364 ) ;
#19517 = CARTESIAN_POINT ( 'NONE',  ( -0.3236067977499789694, 0.3571428571428570398, -0.2351141009169893104 ) ) ;
#19518 = CARTESIAN_POINT ( 'NONE',  ( 0.1306872919485616846, 0.3155070326520292290, 0.4893750000000048894 ) ) ;
#19519 = CYLINDRICAL_SURFACE ( 'NONE', #17668, 0.3119999999999999996 ) ;
#19520 = CARTESIAN_POINT ( 'NONE',  ( 0.4450000000000002842, 0.000000000000000000, -2.540999999999999925 ) ) ;
#19521 = CARTESIAN_POINT ( 'NONE',  ( -0.04084097786787917184, 3.848291582050888948, 0.3120000000000027196 ) ) ;
#19522 = B_SPLINE_CURVE_WITH_KNOTS ( 'NONE', 3,
 ( #16157, #8829, #23689, #7012, #3832, #15056, #7487, #22480, #7724, #8287, #41, #20536 ),
 .UNSPECIFIED., .F., .F.,
 ( 4, 2, 2, 2, 2, 4 ),
 ( 0.000000000000000000, 0.003384026746073580567, 0.006768053492147161135, 0.008460066865183952720, 0.01015208023822074083, 0.01353610698429432574 ),
 .UNSPECIFIED. ) ;
#19523 = CARTESIAN_POINT ( 'NONE',  ( 1.726321361862525858E-17, 0.5493055554796888451, -0.2819296736111110979 ) ) ;
#19524 = CARTESIAN_POINT ( 'NONE',  ( -0.1167790944451423535, 4.099388888964754507, 0.2819296736111110424 ) ) ;
#19525 = CARTESIAN_POINT ( 'NONE',  ( -6.979263641208234666E-17, -0.006250000097542391178, 0.3799334167787516425 ) ) ;
#19526 = CARTESIAN_POINT ( 'NONE',  ( -0.2819296736111110424, 4.641055555631422358, -0.1167790944451423119 ) ) ;
#19527 = LINE ( 'NONE', #17701, #20556 ) ;
#19528 = CARTESIAN_POINT ( 'NONE',  ( 0.02852117301596229088, 5.091364893910177436, -0.3114599212108494775 ) ) ;
#19529 = ORIENTED_EDGE ( 'NONE', *, *, #23811, .T. ) ;
#19530 = ORIENTED_EDGE ( 'NONE', *, *, #19169, .T. ) ;
#19531 = DIRECTION ( 'NONE',  ( -0.000000000000000000, -1.000000000000000000, -0.000000000000000000 ) ) ;
#19532 = CARTESIAN_POINT ( 'NONE',  ( 0.3119999999999999996, 3.752166666818398610, -3.820898013339742174E-17 ) ) ;
#19533 = PLANE ( 'NONE',  #10694 ) ;
#19534 = SHAPE_REPRESENTATION_RELATIONSHIP ( 'NONE' , 'NONE' ,  #18521, #6219 ) ;
#19535 = ORIENTED_EDGE ( 'NONE', *, *, #3824, .F. ) ;
#19536 = CARTESIAN_POINT ( 'NONE',  ( 0.08563601764371561731, 5.206640035683671286, 0.2691675127473932005 ) ) ;
#19537 = DATE_AND_TIME ( #19657, #7256 ) ;
#19538 = ORIENTED_EDGE ( 'NONE', *, *, #14761, .F. ) ;
#19539 = CARTESIAN_POINT ( 'NONE',  ( -0.4805070082343985138, 0.2560807851245828770, 0.04413116910601660309 ) ) ;
#19540 = CARTESIAN_POINT ( 'NONE',  ( -0.1742296017712379186, 4.566445403052646235, 0.2618687473997388104 ) ) ;
#19541 = ORIENTED_EDGE ( 'NONE', *, *, #22229, .T. ) ;
#19542 = CARTESIAN_POINT ( 'NONE',  ( 0.2819296736111110979, -0.006250000075866628431, 0.000000000000000000 ) ) ;
#19543 = ORIENTED_EDGE ( 'NONE', *, *, #5151, .T. ) ;
#19544 = CARTESIAN_POINT ( 'NONE',  ( -5.178964085587577574E-17, 0.09097222214635558579, 0.2819296736111110979 ) ) ;
#19545 = CARTESIAN_POINT ( 'NONE',  ( -0.2616638558779200707, 4.719215415244865319, -0.1714447087179424845 ) ) ;
#19546 = FACE_OUTER_BOUND ( 'NONE', #11207, .T. ) ;
#19547 = CARTESIAN_POINT ( 'NONE',  ( -0.2923287055106771337, 0.3080357141881718275, -0.2123892367102620804 ) ) ;
#19548 = CARTESIAN_POINT ( 'NONE',  ( -0.2283086233831378709, 5.064367125495646604, 0.2126500461812922682 ) ) ;
#19549 = EDGE_CURVE ( 'NONE', #18946, #9548, #19897, .T. ) ;
#19550 = LINE ( 'NONE', #21861, #8854 ) ;
#19551 = CARTESIAN_POINT ( 'NONE',  ( -0.01848103877824600061, -0.5441716683897390716, 0.04413116910601655452 ) ) ;
#19552 = EDGE_CURVE ( 'NONE', #11335, #13239, #4491, .T. ) ;
#19553 = CARTESIAN_POINT ( 'NONE',  ( 0.2819296736111110424, 5.231333333409200037, -0.1167790944451423396 ) ) ;
#19554 = CARTESIAN_POINT ( 'NONE',  ( 0.2719403539735216757, 5.025290946412584780, 0.1583353228916592748 ) ) ;
#19555 = DIRECTION ( 'NONE',  ( 0.000000000000000000, 0.000000000000000000, -1.000000000000000000 ) ) ;
#19556 = CARTESIAN_POINT ( 'NONE',  ( -0.2683823245555305159, 4.775102343486963719, -0.1640186721127107061 ) ) ;
#19557 = CARTESIAN_POINT ( 'NONE',  ( -0.1292346314604057023, 4.568138889040620931, 0.3119999999999998885 ) ) ;
#19558 = EDGE_CURVE ( 'NONE', #20299, #20593, #6386, .T. ) ;
#19559 = CARTESIAN_POINT ( 'NONE',  ( -0.1167790944451423119, 4.689666666742532186, -0.2819296736111110979 ) ) ;
#19560 = VERTEX_POINT ( 'NONE', #20840 ) ;
#19561 = CARTESIAN_POINT ( 'NONE',  ( 0.1993543840281267465, 3.984805555631421470, 0.1993543840281266633 ) ) ;
#19562 = VERTEX_POINT ( 'NONE', #19372 ) ;
#19563 = B_SPLINE_CURVE_WITH_KNOTS ( 'NONE', 3,
 ( #21401, #4929, #679, #15554, #13736, #8223, #13852, #21159, #12036, #15674, #2747, #12158 ),
 .UNSPECIFIED., .F., .F.,
 ( 4, 2, 2, 2, 2, 4 ),
 ( 0.000000000000000000, 0.003384026746073584471, 0.006768053492147168941, 0.008460066865183957924, 0.01015208023822074604, 0.01353610698429432921 ),
 .UNSPECIFIED. ) ;
#19564 = ORIENTED_EDGE ( 'NONE', *, *, #21712, .F. ) ;
#19565 = APPLICATION_PROTOCOL_DEFINITION ( 'international standard', 'config_control_design', 1994, #1411 ) ;
#19566 = CARTESIAN_POINT ( 'NONE',  ( -0.3125000000000000000, 0.1294417382415922468, 0.06402777777777962642 ) ) ;
#19567 = DIRECTION ( 'NONE',  ( 0.000000000000000000, 1.000000000000000000, 0.000000000000000000 ) ) ;
#19568 = CARTESIAN_POINT ( 'NONE',  ( -0.2206173157302027954, 0.08749999984826707655, -0.2206173157302028232 ) ) ;
#19569 = LINE ( 'NONE', #3887, #8163 ) ;
#19570 = CARTESIAN_POINT ( 'NONE',  ( 0.4749999999999999778, 3.575000000000000622, 0.09499999999999998723 ) ) ;
#19571 = CARTESIAN_POINT ( 'NONE',  ( -0.1294417382415922191, 0.3125000000000000000, 0.2793055555555591929 ) ) ;
#19572 = CARTESIAN_POINT ( 'NONE',  ( 0.05068837741648516554, 5.073009555618063438, 0.3078549794868774558 ) ) ;
#19573 = CARTESIAN_POINT ( 'NONE',  ( 9.101228903679513089E-16, 0.3107142857142856096, 0.4000000000000000222 ) ) ;
#19574 = CARTESIAN_POINT ( 'NONE',  ( -3.385114897866767815E-17, -0.2764156081756484196, 0.04666666666666822311 ) ) ;
#19575 = ADVANCED_FACE ( 'NONE', ( #9875 ), #21080, .F. ) ;
#19576 = LINE ( 'NONE', #15688, #20606 ) ;
#19577 = AXIS2_PLACEMENT_3D ( 'NONE', #23707, #5433, #13016 ) ;
#19578 = CARTESIAN_POINT ( 'NONE',  ( -1.726321361862525858E-17, 4.338972222298087544, -0.2819296736111110979 ) ) ;
#19579 = CARTESIAN_POINT ( 'NONE',  ( -0.3129466533217430957, 0.4336677069265437723, -1.132603556623053231 ) ) ;
#19580 = CARTESIAN_POINT ( 'NONE',  ( 1.573500000000000343, 0.5250000000000000222, -0.3524999999999999800 ) ) ;
#19581 = CARTESIAN_POINT ( 'NONE',  ( -1.910449006669871087E-17, 4.870222222222222008, -0.3119999999999999996 ) ) ;
#19582 = CARTESIAN_POINT ( 'NONE',  ( -1.910449006669871087E-17, 4.314666666666665762, -0.3119999999999999996 ) ) ;
#19583 = CARTESIAN_POINT ( 'NONE',  ( -0.3119999999999999996, 5.220916666818399499, -0.1292346314604056468 ) ) ;
#19584 = ADVANCED_FACE ( 'NONE', ( #10119 ), #9916, .T. ) ;
#19585 = CARTESIAN_POINT ( 'NONE',  ( 0.2616181931105792668, 4.969273229293068361, 0.1714232944442920237 ) ) ;
#19586 = DIMENSIONAL_EXPONENTS ( 1.000000000000000000, 0.000000000000000000, 0.000000000000000000, 0.000000000000000000, 0.000000000000000000, 0.000000000000000000, 0.000000000000000000 ) ;
#19587 = CARTESIAN_POINT ( 'NONE',  ( 0.2852966298538977541, 4.581816164709135109, 0.1277710420903920563 ) ) ;
#19588 = ORIENTED_EDGE ( 'NONE', *, *, #4227, .T. ) ;
#19589 =( BOUNDED_CURVE ( )  B_SPLINE_CURVE ( 2, ( #14266, #21703, #15854, #8767, #23632, #23271, #21224, #4513, #15742 ),
 .UNSPECIFIED., .F., .F. ) 
 B_SPLINE_CURVE_WITH_KNOTS ( ( 3, 2, 2, 2, 3 ),
 ( 0.2410714285714287142, 0.2455357142857143293, 0.2499999999999999445, 0.2544642857142855874, 0.2589285714285712303 ),
 .UNSPECIFIED. ) 
 CURVE ( )  GEOMETRIC_REPRESENTATION_ITEM ( )  RATIONAL_B_SPLINE_CURVE ( ( 0.9999999999999976685, 0.9238795325112890700, 1.000000000000000000, 0.9238795325112867385, 1.000000000000000000, 0.9238795325112867385, 1.000000000000000000, 0.9238795325112905132, 0.9999999999999962252 ) ) 
 REPRESENTATION_ITEM ( '' )  );
#19590 = VECTOR ( 'NONE', #11307, 39.37007874015748854 ) ;
#19591 = CARTESIAN_POINT ( 'NONE',  ( 0.2932484408783123109, 4.137880752413645169, 0.1097999344016974271 ) ) ;
#19592 = CARTESIAN_POINT ( 'NONE',  ( 0.2230971623002954429, 0.2230971623002953319, 0.1004861111111132743 ) ) ;
#19593 = CARTESIAN_POINT ( 'NONE',  ( 1.059513921322799533E-10, 3.821611107313654720, -0.3119999999999999996 ) ) ;
#19594 = EDGE_CURVE ( 'NONE', #19238, #5827, #9138, .T. ) ;
#19595 = CARTESIAN_POINT ( 'NONE',  ( -0.1116596296178200276, 0.2580357141881718941, 0.3436530038418508792 ) ) ;
#19596 = ADVANCED_FACE ( 'NONE', ( #6680 ), #7052, .T. ) ;
#19597 = ADVANCED_FACE ( 'NONE', ( #6927 ), #21554, .T. ) ;
#19598 = CARTESIAN_POINT ( 'NONE',  ( 0.1993543840281266910, 0.5979166665908001166, -0.1993543840281266910 ) ) ;
#19599 = CARTESIAN_POINT ( 'NONE',  ( 0.2764156081756483641, -0.1144950937579611167, 0.1195833333333354426 ) ) ;
#19600 = CARTESIAN_POINT ( 'NONE',  ( 0.1891708636127259202, 2.539511724522405989E-17, 0.3078630284654709781 ) ) ;
#19601 = CARTESIAN_POINT ( 'NONE',  ( -0.003401740878768693549, 0.5383620901250332214, 0.05893285591566552878 ) ) ;
#19602 = CARTESIAN_POINT ( 'NONE',  ( -0.1954553509668046640, 0.1954553509668046918, 0.4216666666666711305 ) ) ;
#19603 = ORIENTED_EDGE ( 'NONE', *, *, #16641, .T. ) ;
#19604 = CARTESIAN_POINT ( 'NONE',  ( -0.6209078282299125284, 7.622621636232170019E-17, -0.01219352927422984872 ) ) ;
#19605 = CARTESIAN_POINT ( 'NONE',  ( -0.07708971822763990844, 4.291625973313240472, 0.3029365359921079581 ) ) ;
#19606 = DIRECTION ( 'NONE',  ( 0.000000000000000000, 0.000000000000000000, -1.000000000000000000 ) ) ;
#19607 = CARTESIAN_POINT ( 'NONE',  ( -5.731347020009612645E-17, 0.3930555555555551583, 0.3119999999999999996 ) ) ;
#19608 = CARTESIAN_POINT ( 'NONE',  ( 0.1292346314604056190, 4.922305555555555046, -0.3119999999999999996 ) ) ;
#19609 = CARTESIAN_POINT ( 'NONE',  ( -0.2819296736111110979, 4.241750000075865223, 0.000000000000000000 ) ) ;
#19610 = AXIS2_PLACEMENT_3D ( 'NONE', #13577, #865, #10032 ) ;
#19611 = CARTESIAN_POINT ( 'NONE',  ( -0.1167790944451423535, 4.043833333409200037, 0.2819296736111110424 ) ) ;
#19612 = ADVANCED_FACE ( 'NONE', ( #10357 ), #21795, .T. ) ;
#19613 = CARTESIAN_POINT ( 'NONE',  ( -5.731347020009612645E-17, 0.6083333331816004330, 0.3119999999999999996 ) ) ;
#19614 = CARTESIAN_POINT ( 'NONE',  ( -1.910449006669871087E-17, 3.870222222222221564, -0.3119999999999999996 ) ) ;
#19615 = CARTESIAN_POINT ( 'NONE',  ( 0.3115568539166290729, 4.807258945525052951, 0.01709936015787908575 ) ) ;
#19616 = EDGE_LOOP ( 'NONE', ( #22729, #11556, #24019, #5863 ) ) ;
#19617 = DIRECTION ( 'NONE',  ( 0.000000000000000000, -0.2142211582677938930, -0.9767851838303059919 ) ) ;
#19618 = CARTESIAN_POINT ( 'NONE',  ( 0.1167790944451422702, 4.502166666742532186, -0.2819296736111110424 ) ) ;
#19619 = CARTESIAN_POINT ( 'NONE',  ( -0.02692592971120469358, 4.515319170270573501, 0.3108360067888585876 ) ) ;
#19620 = PERSON_AND_ORGANIZATION ( #15518, #2538 ) ;
#19621 = CARTESIAN_POINT ( 'NONE',  ( -0.4687500000000003886, -0.2598076211353319009, 0.06112444011295370405 ) ) ;
#19622 = CARTESIAN_POINT ( 'NONE',  ( -0.1144950937579609918, -0.2764156081756484196, 0.04319444444444596465 ) ) ;
#19623 = LINE ( 'NONE', #1094, #10005 ) ;
#19624 = CARTESIAN_POINT ( 'NONE',  ( -1.726321361862525858E-17, 4.130638888964754507, -0.2819296736111110979 ) ) ;
#19625 = CIRCLE ( 'NONE', #20038, 0.2501339745962155581 ) ;
#19626 = CARTESIAN_POINT ( 'NONE',  ( 2.781172880863639385E-17, 0.000000000000000000, -0.2041999999999999926 ) ) ;
#19627 = LINE ( 'NONE', #2923, #18740 ) ;
#19628 = CARTESIAN_POINT ( 'NONE',  ( -3.385114897866767815E-17, -0.2764156081756484196, 0.2202777777777806811 ) ) ;
#19629 = CARTESIAN_POINT ( 'NONE',  ( 0.3613381517857143232, 0.1508928570453146878, 0.1174058825155742114 ) ) ;
#19630 = CARTESIAN_POINT ( 'NONE',  ( -0.1167790944451422702, 0.05277777770191114520, -0.2819296736111110424 ) ) ;
#19631 = CARTESIAN_POINT ( 'NONE',  ( 0.4687500000000003331, -0.08694941101440553655, 0.07654963157453610612 ) ) ;
#19632 = CARTESIAN_POINT ( 'NONE',  ( -0.4800179188494136939, 0.1716492620570552741, 0.06108894518741068980 ) ) ;
#19633 = DIRECTION ( 'NONE',  ( 0.000000000000000000, 0.000000000000000000, 1.000000000000000000 ) ) ;
#19634 = DIRECTION ( 'NONE',  ( 0.000000000000000000, 0.000000000000000000, 1.000000000000000000 ) ) ;
#19635 = CARTESIAN_POINT ( 'NONE',  ( -0.2230971623002954152, -0.2230971623002953874, 0.2914583333333366499 ) ) ;
#19636 = DIRECTION ( 'NONE',  ( -0.000000000000000000, 1.000000000000000000, -0.000000000000000000 ) ) ;
#19637 = DIRECTION ( 'NONE',  ( 0.6681584153635196088, -0.6681584153635196088, -0.3273051541876794701 ) ) ;
#19638 = CARTESIAN_POINT ( 'NONE',  ( 0.000000000000000000, 2.735000000000000320, 0.000000000000000000 ) ) ;
#19639 = AXIS2_PLACEMENT_3D ( 'NONE', #7922, #15253, #15376 ) ;
#19640 = CARTESIAN_POINT ( 'NONE',  ( 0.2819296736111110424, 0.4833333332574667462, -0.1167790944451423119 ) ) ;
#19641 = CARTESIAN_POINT ( 'NONE',  ( -0.1993543840281266910, 4.026472222298087544, -0.1993543840281266910 ) ) ;
#19642 = CARTESIAN_POINT ( 'NONE',  ( 0.3613381517857143232, 0.08660714275960043618, -0.1174058825155740587 ) ) ;
#19643 = EDGE_CURVE ( 'NONE', #17146, #5661, #12431, .T. ) ;
#19644 = ORIENTED_EDGE ( 'NONE', *, *, #15276, .F. ) ;
#19645 = CARTESIAN_POINT ( 'NONE',  ( 0.1993543840281267465, 4.609805555631421470, 0.1993543840281266633 ) ) ;
#19646 = PRODUCT ( 'Aloris-BXA-Center-Rod', 'Aloris-BXA-Center-Rod', '', ( #4863 ) ) ;
#19647 = DIRECTION ( 'NONE',  ( -1.000000000000000000, 0.000000000000000000, 0.000000000000000000 ) ) ;
#19648 = CARTESIAN_POINT ( 'NONE',  ( 0.2991168607796587109, 5.081043917475041027, -0.08951420082251353161 ) ) ;
#19649 = ORIENTED_EDGE ( 'NONE', *, *, #17286, .T. ) ;
#19650 = CARTESIAN_POINT ( 'NONE',  ( -0.3125000000000004441, 0.1294417382415918583, 0.3973611111111156613 ) ) ;
#19651 = CARTESIAN_POINT ( 'NONE',  ( 0.1167790944451422702, 5.224388888964754507, -0.2819296736111110424 ) ) ;
#19652 = AXIS2_PLACEMENT_3D ( 'NONE', #14088, #10317, #17500 ) ;
#19653 = CARTESIAN_POINT ( 'NONE',  ( 1.573500000000000343, -3.414809992080329023E-17, -0.1400000000000000133 ) ) ;
#19654 = FACE_OUTER_BOUND ( 'NONE', #22185, .T. ) ;
#19655 = CC_DESIGN_SECURITY_CLASSIFICATION ( #12686, ( #11902 ) ) ;
#19656 = CARTESIAN_POINT ( 'NONE',  ( -0.1993543840281266355, 4.859805555631421470, 0.1993543840281267465 ) ) ;
#19657 = CALENDAR_DATE ( 2026, 7, 10 ) ;
#19658 = VERTEX_POINT ( 'NONE', #4845 ) ;
#19659 = CARTESIAN_POINT ( 'NONE',  ( -0.1885148968005289083, 5.106211064497114371, -0.2472071745827196798 ) ) ;
#19660 = CARTESIAN_POINT ( 'NONE',  ( -0.04622711050593557303, 4.570331327651010689, 0.3085716787575049636 ) ) ;
#19661 = ORIENTED_EDGE ( 'NONE', *, *, #1859, .T. ) ;
#19662 = CARTESIAN_POINT ( 'NONE',  ( -0.2819296736111110979, 0.3583333332574666907, 0.1167790944451422425 ) ) ;
#19663 = VERTEX_POINT ( 'NONE', #3143 ) ;
#19664 = DIRECTION ( 'NONE',  ( 0.000000000000000000, 0.2773500981126134080, -0.9607689228305230644 ) ) ;
#19665 = CARTESIAN_POINT ( 'NONE',  ( -0.1292346314604058410, 0.3340277777777773682, 0.3119999999999998885 ) ) ;
#19666 = CARTESIAN_POINT ( 'NONE',  ( 0.000000000000000000, 0.000000000000000000, 0.4425000000000000044 ) ) ;
#19667 = VECTOR ( 'NONE', #12941, 39.37007874015748143 ) ;
#19668 = CARTESIAN_POINT ( 'NONE',  ( -0.1116596296178200276, 0.3294642856167432354, 0.3436530038418508792 ) ) ;
#19669 = CARTESIAN_POINT ( 'NONE',  ( -0.1292346314604020385, 4.505638888888888083, 0.3120000000000036078 ) ) ;
#19670 = LINE ( 'NONE', #18206, #13167 ) ;
#19671 = CARTESIAN_POINT ( 'NONE',  ( -0.3143659348029792522, -0.3723832402019556231, 0.07159583130656665961 ) ) ;
#19672 = CARTESIAN_POINT ( 'NONE',  ( 0.2819296736111110979, 3.769527777853642903, -3.452642723725051716E-17 ) ) ;
#19673 = CARTESIAN_POINT ( 'NONE',  ( -0.2978458783688814338, 0.05116650193037295541, -0.04224598531790686035 ) ) ;
#19674 = LINE ( 'NONE', #13839, #18800 ) ;
#19675 = DIRECTION ( 'NONE',  ( 0.000000000000000000, -0.000000000000000000, -1.000000000000000000 ) ) ;
#19676 = CARTESIAN_POINT ( 'NONE',  ( 4.589422455927707524E-07, 4.793851445074613693, 0.3119999999992840167 ) ) ;
#19677 = CARTESIAN_POINT ( 'NONE',  ( -0.3119999999999999996, 4.609805555707287006, -0.1292346314604056468 ) ) ;
#19678 = CARTESIAN_POINT ( 'NONE',  ( 0.2819296736111110979, 4.783416666742532186, -3.452642723725051716E-17 ) ) ;
#19679 = VERTEX_POINT ( 'NONE', #3259 ) ;
#19680 = CARTESIAN_POINT ( 'NONE',  ( -1.726321361862525858E-17, 4.061194444520309865, -0.2819296736111110979 ) ) ;
#19681 = VECTOR ( 'NONE', #16769, 39.37007874015748854 ) ;
#19682 = ORIENTED_EDGE ( 'NONE', *, *, #7509, .F. ) ;
#19683 = EDGE_CURVE ( 'NONE', #23806, #11205, #15681, .T. ) ;
#19684 = DATE_AND_TIME ( #14086, #6041 ) ;
#19685 = VERTEX_POINT ( 'NONE', #23248 ) ;
#19686 = FACE_OUTER_BOUND ( 'NONE', #1491, .T. ) ;
#19687 = CARTESIAN_POINT ( 'NONE',  ( 0.5237631043874195758, 2.661358883302036293, -0.6748402668043530506 ) ) ;
#19688 = ORGANIZATION ( 'NAUO-ORG2', 'UNSPECIFIED', 'UNSPECIFIED' ) ;
#19689 = ORIENTED_EDGE ( 'NONE', *, *, #17114, .T. ) ;
#19690 = CARTESIAN_POINT ( 'NONE',  ( -0.2206173157302027954, 0.03194444429271151714, -0.2206173157302028232 ) ) ;
#19691 = CARTESIAN_POINT ( 'NONE',  ( -0.2337193498271271375, 4.384649860946254307, -0.2067694730596380537 ) ) ;
#19692 = CC_DESIGN_PERSON_AND_ORGANIZATION_ASSIGNMENT ( #7603, #1999, ( #4115 ) ) ;
#19693 = CARTESIAN_POINT ( 'NONE',  ( 0.2206173157302028232, 0.1847222220704893003, -0.2206173157302028232 ) ) ;
#19694 = DIRECTION ( 'NONE',  ( 0.4999999999999913403, 0.000000000000000000, 0.8660254037844434816 ) ) ;
#19695 = ORIENTED_EDGE ( 'NONE', *, *, #8725, .T. ) ;
#19696 = CLOSED_SHELL ( 'NONE', ( #4355, #18883, #5291, #3168, #13256, #9602, #16626, #7287, #11624, #4109, #6371, #12620, #6887, #17233, #6313, #4417, #9179, #2096, #22522, #14378, #7392, #2584, #13762, #21205, #126, #5162, #4358, #8135, #1916, #9472, #4245, #19575, #12670, #9868, #10227, #11357, #7427, #18245, #23162 ) ) ;
#19697 = CARTESIAN_POINT ( 'NONE',  ( 2.122261530980286359, 2.737827333818739106, -2.942657555934166780 ) ) ;
#19698 = CARTESIAN_POINT ( 'NONE',  ( 1.109470958122166229, 2.291712385858714285, -1.012998853824579104 ) ) ;
#19699 = CARTESIAN_POINT ( 'NONE',  ( 0.2764156081756483641, -0.1144950937579611167, 0.1126388888888909395 ) ) ;
#19700 = CARTESIAN_POINT ( 'NONE',  ( -0.2819296736111110424, 4.356333333409198261, 0.1167790944451424923 ) ) ;
#19701 = CARTESIAN_POINT ( 'NONE',  ( 0.4795759075923620163, -5.969813580926603513E-13, 0.07439896364136204532 ) ) ;
#19702 = CARTESIAN_POINT ( 'NONE',  ( -7.331754493858430024E-07, 4.349360015129621004, 0.3119999999981767358 ) ) ;
#19703 = DIRECTION ( 'NONE',  ( -0.000000000000000000, -1.000000000000000000, -0.000000000000000000 ) ) ;
#19704 = CARTESIAN_POINT ( 'NONE',  ( 2.296137995767620676, 2.978485840173427324, -2.088288568297006265 ) ) ;
#19705 = CARTESIAN_POINT ( 'NONE',  ( -0.1292346314604057023, 4.005638888888888971, 0.3119999999999998885 ) ) ;
#19706 = CARTESIAN_POINT ( 'NONE',  ( -0.3119999999999999996, 5.109805555707287894, -0.1292346314604056468 ) ) ;
#19707 = DIRECTION ( 'NONE',  ( 0.000000000000000000, 0.000000000000000000, 1.000000000000000000 ) ) ;
#19708 = SECURITY_CLASSIFICATION ( '', '', #5135 ) ;
#19709 = VERTEX_POINT ( 'NONE', #2899 ) ;
#19710 = CARTESIAN_POINT ( 'NONE',  ( 0.4700000000000000844, 2.740000000000000213, 8.024803481388775053E-17 ) ) ;
#19711 = ORIENTED_EDGE ( 'NONE', *, *, #199, .T. ) ;
#19712 = CARTESIAN_POINT ( 'NONE',  ( -0.3125000000000000000, 1.913510623667739771E-17, 0.2341666666666698537 ) ) ;
#19713 = VECTOR ( 'NONE', #13155, 39.37007874015748143 ) ;
#19714 = CARTESIAN_POINT ( 'NONE',  ( 0.2230971623002954429, 0.2230971623002953319, -0.01062499999999870839 ) ) ;
#19715 = DIRECTION ( 'NONE',  ( -0.5000000000000003331, 0.000000000000000000, -0.8660254037844384856 ) ) ;
#19716 = CARTESIAN_POINT ( 'NONE',  ( -0.1292346314604008173, 4.450083333333332725, 0.3120000000000048845 ) ) ;
#19717 = EDGE_CURVE ( 'NONE', #22559, #10294, #18855, .T. ) ;
#19718 = CARTESIAN_POINT ( 'NONE',  ( -0.2923287055106771337, 0.1794642856167432687, 0.2123892367102619971 ) ) ;
#19719 = CARTESIAN_POINT ( 'NONE',  ( 0.1993543840281266910, 0.05624999992413336897, -0.1993543840281266910 ) ) ;
#19720 = CARTESIAN_POINT ( 'NONE',  ( 0.1954553509668047195, 0.1954553509668046085, 0.07444444444444621445 ) ) ;
#19721 = DIRECTION ( 'NONE',  ( 0.4472135954999557628, 0.4472135954999557628, 0.7745966692414858468 ) ) ;
#19722 = CARTESIAN_POINT ( 'NONE',  ( 0.1993543840281266633, 5.179250000075866112, -0.1993543840281266910 ) ) ;
#19723 = CARTESIAN_POINT ( 'NONE',  ( 0.1144950937579611444, 0.2764156081756483641, 0.4112500000000043898 ) ) ;
#19724 = ORIENTED_EDGE ( 'NONE', *, *, #16016, .F. ) ;
#19725 = CARTESIAN_POINT ( 'NONE',  ( 2.802071455580988509E-07, 4.599388881221821990, -0.3119999999998741003 ) ) ;
#19726 = CARTESIAN_POINT ( 'NONE',  ( -0.002160124341594215833, 4.293772033077872585, 0.3119935960890014570 ) ) ;
#19727 = CARTESIAN_POINT ( 'NONE',  ( 3.061616997868383634E-17, 0.4199999999999998734, -0.2500000000000000555 ) ) ;
#19728 = CARTESIAN_POINT ( 'NONE',  ( 0.3119999999999999996, 0.5215277777777774793, -0.1292346314604056468 ) ) ;
#19729 = CARTESIAN_POINT ( 'NONE',  ( 0.2206173157302028787, 4.904944444444443441, 0.2206173157302027954 ) ) ;
#19730 = VECTOR ( 'NONE', #10617, 39.37007874015748143 ) ;
#19731 = CARTESIAN_POINT ( 'NONE',  ( 0.2819296736111110979, 4.328555555631421470, -0.1167790944451423396 ) ) ;
#19732 = CARTESIAN_POINT ( 'NONE',  ( -0.1167790944451423535, 3.932722222298087544, 0.2819296736111110424 ) ) ;
#19733 =( BOUNDED_CURVE ( )  B_SPLINE_CURVE ( 2, ( #18329, #1741, #16264, #20037, #3207, #24045, #5154, #16140, #23797 ),
 .UNSPECIFIED., .F., .T. ) 
 B_SPLINE_CURVE_WITH_KNOTS ( ( 3, 2, 2, 2, 3 ),
 ( 0.3541666666666666852, 0.3645833333333333148, 0.3750000000000000000, 0.3854166666666666852, 0.3958333333333333148 ),
 .UNSPECIFIED. ) 
 CURVE ( )  GEOMETRIC_REPRESENTATION_ITEM ( )  RATIONAL_B_SPLINE_CURVE ( ( 1.000000000000000000, 0.9238795325112867385, 1.000000000000000000, 0.9238795325112867385, 1.000000000000000000, 0.9238795325112867385, 1.000000000000000000, 0.9238795325112867385, 1.000000000000000000 ) ) 
 REPRESENTATION_ITEM ( '' )  );
#19734 = CARTESIAN_POINT ( 'NONE',  ( -0.3120000000000000551, 0.5979166665149336923, 0.1292346314604056190 ) ) ;
#19735 = CARTESIAN_POINT ( 'NONE',  ( -0.3838430204063939533, 0.3081239094298380832, 0.4164750180373177346 ) ) ;
#19736 = CARTESIAN_POINT ( 'NONE',  ( 1.312321497832610059E-07, 4.821611112096344520, -0.3119999999999724105 ) ) ;
#19737 =( BOUNDED_CURVE ( )  B_SPLINE_CURVE ( 2, ( #14061, #19904, #1250, #17957, #3083, #10640, #6735, #1372, #16006 ),
 .UNSPECIFIED., .F., .F. ) 
 B_SPLINE_CURVE_WITH_KNOTS ( ( 3, 2, 2, 2, 3 ),
 ( 0.2708333333333333148, 0.2812500000000000000, 0.2916666666666666852, 0.3020833333333333148, 0.3125000000000000000 ),
 .UNSPECIFIED. ) 
 CURVE ( )  GEOMETRIC_REPRESENTATION_ITEM ( )  RATIONAL_B_SPLINE_CURVE ( ( 1.000000000000000000, 0.9238795325112867385, 1.000000000000000000, 0.9238795325112867385, 1.000000000000000000, 0.9238795325112867385, 1.000000000000000000, 0.9238795325112867385, 1.000000000000000000 ) ) 
 REPRESENTATION_ITEM ( '' )  );
#19738 = ORIENTED_EDGE ( 'NONE', *, *, #17634, .F. ) ;
#19739 = CARTESIAN_POINT ( 'NONE',  ( -0.2726213665948679643, 4.006868641008068721, 0.1571290981393282105 ) ) ;
#19740 = CARTESIAN_POINT ( 'NONE',  ( -0.1167790944451423257, 4.398000000075866112, -0.2819296736111110424 ) ) ;
#19741 = CARTESIAN_POINT ( 'NONE',  ( -0.2999751848458688253, 4.499730033197880452, -0.08647106361988687873 ) ) ;
#19742 = EDGE_CURVE ( 'NONE', #11791, #15529, #17302, .T. ) ;
#19743 = EDGE_CURVE ( 'NONE', #12281, #4326, #20576, .T. ) ;
#19744 = APPLICATION_PROTOCOL_DEFINITION ( 'international standard', 'config_control_design', 1994, #16368 ) ;
#19745 = CARTESIAN_POINT ( 'NONE',  ( 0.3834923435458895136, 0.3083291687941427939, 0.4165495381634259364 ) ) ;
#19746 = CARTESIAN_POINT ( 'NONE',  ( 0.2764156081756484196, -5.077672346800151106E-17, 0.005000000000001210074 ) ) ;
#19747 = AXIS2_PLACEMENT_3D ( 'NONE', #23108, #11931, #19350 ) ;
#19748 = DIMENSIONAL_EXPONENTS ( 1.000000000000000000, 0.000000000000000000, 0.000000000000000000, 0.000000000000000000, 0.000000000000000000, 0.000000000000000000, 0.000000000000000000 ) ;
#19749 = CARTESIAN_POINT ( 'NONE',  ( -0.2819296736111110979, 4.141055555631421470, -0.1167790944451422980 ) ) ;
#19750 = COORDINATED_UNIVERSAL_TIME_OFFSET ( 0, 0, .AHEAD. ) ;
#19751 = CARTESIAN_POINT ( 'NONE',  ( -0.3119999999999999996, 0.3791666666666663188, -3.820898013339742174E-17 ) ) ;
#19752 = EDGE_CURVE ( 'NONE', #5871, #2851, #16141, .T. ) ;
#19753 = DIRECTION ( 'NONE',  ( 0.000000000000000000, 0.000000000000000000, -1.000000000000000000 ) ) ;
#19754 = CARTESIAN_POINT ( 'NONE',  ( 0.1954553509668047195, 0.1954553509668046085, 0.1855555555555581937 ) ) ;
#19755 = CARTESIAN_POINT ( 'NONE',  ( 2.326421213736078119E-17, -0.04196428581182810869, -0.3799334167787516425 ) ) ;
#19756 = CARTESIAN_POINT ( 'NONE',  ( 0.1167790944451423535, 0.5944444443685777957, 0.2819296736111110424 ) ) ;
#19757 = CARTESIAN_POINT ( 'NONE',  ( -0.4749999999999999778, 3.575000000000000622, 0.09499999999999995948 ) ) ;
#19758 = DIRECTION ( 'NONE',  ( 0.000000000000000000, 0.7071067811865474617, 0.7071067811865474617 ) ) ;
#19759 = CARTESIAN_POINT ( 'NONE',  ( -0.02831565414742191061, 0.5908090236396409400, -0.7495925827047090761 ) ) ;
#19760 = CARTESIAN_POINT ( 'NONE',  ( -0.1144950937579609918, -0.2764156081756484196, 0.09875000000000197509 ) ) ;
#19761 = CARTESIAN_POINT ( 'NONE',  ( 0.3155070326520292290, -0.1306872919485616569, 0.3088194444444478659 ) ) ;
#19762 = EDGE_LOOP ( 'NONE', ( #15790, #22268, #22196, #21019 ) ) ;
#19763 = DIRECTION ( 'NONE',  ( -0.000000000000000000, -1.000000000000000000, -0.000000000000000000 ) ) ;
#19764 = CARTESIAN_POINT ( 'NONE',  ( 0.4584466503968441797, 0.2219868246720123339, 0.4062958900596150280 ) ) ;
#19765 = CARTESIAN_POINT ( 'NONE',  ( 0.1167790944451423257, 0.4902777777019112215, -0.2819296736111110424 ) ) ;
#19766 = CARTESIAN_POINT ( 'NONE',  ( -0.1993543840281266355, 3.984805555631421470, 0.1993543840281267465 ) ) ;
#19767 = CARTESIAN_POINT ( 'NONE',  ( -0.2233192592356399997, -0.01339285724039953294, 0.3073725909049499494 ) ) ;
#19768 = ORIENTED_EDGE ( 'NONE', *, *, #3042, .T. ) ;
#19769 = CARTESIAN_POINT ( 'NONE',  ( -0.2819296736111110979, 4.588972222298088433, 0.000000000000000000 ) ) ;
#19770 = CARTESIAN_POINT ( 'NONE',  ( 0.2491934408984518567, 5.125924046562484016, 0.1804089006109781124 ) ) ;
#19771 = EDGE_CURVE ( 'NONE', #22186, #12538, #3304, .T. ) ;
#19772 = CARTESIAN_POINT ( 'NONE',  ( 0.000000000000000000, 3.700000000000000622, -0.3125000000000000000 ) ) ;
#19773 = ORIENTED_EDGE ( 'NONE', *, *, #4443, .T. ) ;
#19774 = AXIS2_PLACEMENT_3D ( 'NONE', #10994, #23889, #9396 ) ;
#19775 = CARTESIAN_POINT ( 'NONE',  ( 0.3119999999999999996, 4.026472222222221120, -0.1292346314604056745 ) ) ;
#19776 = CARTESIAN_POINT ( 'NONE',  ( 5.178964085587577574E-17, 5.088972222298087544, 0.2819296736111110979 ) ) ;
#19777 = CARTESIAN_POINT ( 'NONE',  ( 0.2646253146636260434, 4.191643205751345747, 0.1652801019260927984 ) ) ;
#19778 = CARTESIAN_POINT ( 'NONE',  ( 0.09911565489844109678, 0.03242967361111059182, 0.2643245622819848095 ) ) ;
#19779 = CARTESIAN_POINT ( 'NONE',  ( 0.2819296736111111534, 4.988277777853643791, 0.1167790944451422563 ) ) ;
#19780 = PERSON_AND_ORGANIZATION ( #15518, #2538 ) ;
#19781 = ORIENTED_EDGE ( 'NONE', *, *, #11886, .T. ) ;
#19782 = CARTESIAN_POINT ( 'NONE',  ( -0.09954347264555452046, 5.103090623246006707, -0.2948505828934365747 ) ) ;
#19783 = DIRECTION ( 'NONE',  ( 0.000000000000000000, -0.000000000000000000, -1.000000000000000000 ) ) ;
#19784 = ORIENTED_EDGE ( 'NONE', *, *, #61, .T. ) ;
#19785 = CARTESIAN_POINT ( 'NONE',  ( 0.1993543840281266910, 0.2229166665908000333, -0.1993543840281266910 ) ) ;
#19786 = CIRCLE ( 'NONE', #1873, 0.3150000000000000022 ) ;
#19787 = EDGE_LOOP ( 'NONE', ( #19329, #5751 ) ) ;
#19788 = CARTESIAN_POINT ( 'NONE',  ( -0.4500000000000003997, -0.2598076211353319009, 0.3779506566538942125 ) ) ;
#19789 = FACE_OUTER_BOUND ( 'NONE', #15787, .T. ) ;
#19790 = CARTESIAN_POINT ( 'NONE',  ( 0.04216970674995203922, 4.098166857964845811, -0.3119999999999987228 ) ) ;
#19791 = CARTESIAN_POINT ( 'NONE',  ( -6.979263641208234666E-17, 0.2616071427596003973, 0.3799334167787516425 ) ) ;
#19792 = CARTESIAN_POINT ( 'NONE',  ( -0.2930162582832894214, 5.060969273910194133, 0.1096452931246931495 ) ) ;
#19793 = DIRECTION ( 'NONE',  ( 0.000000000000000000, 1.000000000000000000, 0.000000000000000000 ) ) ;
#19794 = DIRECTION ( 'NONE',  ( -0.4985709748471497393, -0.07555085810113111588, -0.8635502596144276621 ) ) ;
#19795 = CARTESIAN_POINT ( 'NONE',  ( 0.1993543840281266633, 4.623694444520309865, -0.1993543840281266910 ) ) ;
#19796 = ORIENTED_EDGE ( 'NONE', *, *, #2715, .T. ) ;
#19797 = CARTESIAN_POINT ( 'NONE',  ( -0.1649704474213682104, -0.4586382700592834261, 0.07155713030921624640 ) ) ;
#19798 = CARTESIAN_POINT ( 'NONE',  ( -0.1167790944451423257, 3.731333333409198261, -0.2819296736111110424 ) ) ;
#19799 = CARTESIAN_POINT ( 'NONE',  ( -0.2207274099297822922, 0.04780226632771114592, -0.1994142295682237720 ) ) ;
#19800 = CARTESIAN_POINT ( 'NONE',  ( -0.3119999999999999996, 0.09444444429271151020, -3.820898013339742174E-17 ) ) ;
#19801 = DIRECTION ( 'NONE',  ( -0.000000000000000000, -1.000000000000000000, -0.000000000000000000 ) ) ;
#19802 = CARTESIAN_POINT ( 'NONE',  ( -0.05023616953324346046, 4.792438398584838666, 0.3079329440659664963 ) ) ;
#19803 = CARTESIAN_POINT ( 'NONE',  ( 0.3119999999999999996, 4.363277777929510215, -3.820898013339742174E-17 ) ) ;
#19804 = CARTESIAN_POINT ( 'NONE',  ( -0.1167790944451423535, 4.766055555631421470, 0.2819296736111110979 ) ) ;
#19805 = ORIENTED_EDGE ( 'NONE', *, *, #17380, .T. ) ;
#19806 = CARTESIAN_POINT ( 'NONE',  ( -0.1993543840281266355, 3.859805555631421026, 0.1993543840281267465 ) ) ;
#19807 = VECTOR ( 'NONE', #9567, 39.37007874015748143 ) ;
#19808 = ORIENTED_EDGE ( 'NONE', *, *, #17365, .T. ) ;
#19809 = ORIENTED_EDGE ( 'NONE', *, *, #16976, .T. ) ;
#19810 = DATE_AND_TIME ( #12393, #3330 ) ;
#19811 = EDGE_CURVE ( 'NONE', #15879, #23116, #18175, .T. ) ;
#19812 = DIRECTION ( 'NONE',  ( 0.000000000000000000, 0.000000000000000000, -1.000000000000000000 ) ) ;
#19813 = DIRECTION ( 'NONE',  ( 0.000000000000000000, 1.000000000000000000, 0.000000000000000000 ) ) ;
#19814 = ORIENTED_EDGE ( 'NONE', *, *, #14453, .F. ) ;
#19815 = CARTESIAN_POINT ( 'NONE',  ( -0.3119999999999999996, 0.3722222220704893281, -3.820898013339742174E-17 ) ) ;
#19816 = CARTESIAN_POINT ( 'NONE',  ( -0.2804777715993982956, 4.387060150774842349, -0.1381842819380600940 ) ) ;
#19817 = FACE_OUTER_BOUND ( 'NONE', #21199, .T. ) ;
#19818 = CARTESIAN_POINT ( 'NONE',  ( 2.114905110478964667E-17, 0.5924045552181390617, -0.7500000000000001110 ) ) ;
#19819 = ORIENTED_EDGE ( 'NONE', *, *, #6032, .F. ) ;
#19820 = AXIS2_PLACEMENT_3D ( 'NONE', #9174, #5268, #1735 ) ;
#19821 = EDGE_LOOP ( 'NONE', ( #15394, #6787, #288, #7183 ) ) ;
#19822 = DIRECTION ( 'NONE',  ( -0.000000000000000000, -1.000000000000000000, -0.000000000000000000 ) ) ;
#19823 = CARTESIAN_POINT ( 'NONE',  ( 0.000000000000000000, 5.954200000000001936, -0.2500000000000000000 ) ) ;
#19824 = CARTESIAN_POINT ( 'NONE',  ( 0.1954553509668047195, 0.1954553509668046085, 0.01194444444444571485 ) ) ;
#19825 = CARTESIAN_POINT ( 'NONE',  ( -0.1993543840281266910, 4.457027777853642903, -0.1993543840281266910 ) ) ;
#19826 = CARTESIAN_POINT ( 'NONE',  ( -0.1294417382415922746, -0.3125000000000000000, 0.4043055555555598035 ) ) ;
#19827 = CARTESIAN_POINT ( 'NONE',  ( -0.3149849110527242479, 0.4935441587820288967, -1.115363383729591540 ) ) ;
#19828 = CARTESIAN_POINT ( 'NONE',  ( -3.345742422185251127E-06, 4.766055647721512578, -0.3119999999820609049 ) ) ;
#19829 = CARTESIAN_POINT ( 'NONE',  ( -0.1568911027456994511, 4.215120699763493128, -0.2727482857155890117 ) ) ;
#19830 = CARTESIAN_POINT ( 'NONE',  ( -1.910449006669871087E-17, 4.036888888888888083, -0.3119999999999999996 ) ) ;
#19831 = CARTESIAN_POINT ( 'NONE',  ( -0.1292346314604057023, 4.901472222373953969, 0.3119999999999998885 ) ) ;
#19832 = ORIENTED_EDGE ( 'NONE', *, *, #20607, .T. ) ;
#19833 = CARTESIAN_POINT ( 'NONE',  ( -0.03213320543484096681, 4.878081089662273939, -0.3105925309973510684 ) ) ;
#19834 = CARTESIAN_POINT ( 'NONE',  ( 0.2230971623002954429, 0.2230971623002953319, -0.06618055555555471536 ) ) ;
#19835 = CARTESIAN_POINT ( 'NONE',  ( 0.1167790944451422702, 5.224388888964754507, -0.2819296736111110424 ) ) ;
#19836 = CARTESIAN_POINT ( 'NONE',  ( 0.1917385266880204386, 3.799560276120441227, 0.2494960911888102484 ) ) ;
#19837 = PRODUCT ( 'MAS-409-Body', 'MAS-409-Body', '', ( #10412 ) ) ;
#19838 = CARTESIAN_POINT ( 'NONE',  ( 0.3613381517857143232, 0.2794642856167433020, 0.000000000000000000 ) ) ;
#19839 = DIRECTION ( 'NONE',  ( 1.000000000000000000, 0.000000000000000000, 0.000000000000000000 ) ) ;
#19840 = CARTESIAN_POINT ( 'NONE',  ( 0.2764156081756483641, 0.1144950937579610056, 0.07097222222222394905 ) ) ;
#19841 = CARTESIAN_POINT ( 'NONE',  ( 0.1167790944451424368, 5.217444444520309865, 0.2819296736111110424 ) ) ;
#19842 = CARTESIAN_POINT ( 'NONE',  ( 0.1144950937579609085, -0.2764156081756484751, 0.3348611111111148841 ) ) ;
#19843 = ORIENTED_EDGE ( 'NONE', *, *, #5875, .F. ) ;
#19844 = CARTESIAN_POINT ( 'NONE',  ( -0.02506413332034217525, 4.600113615547450685, -0.3110320965815868144 ) ) ;
#19845 = VECTOR ( 'NONE', #20657, 39.37007874015748143 ) ;
#19846 = FACE_BOUND ( 'NONE', #5417, .T. ) ;
#19847 = CARTESIAN_POINT ( 'NONE',  ( 0.000000000000000000, 0.000000000000000000, 1.326383476483184332 ) ) ;
#19848 = CARTESIAN_POINT ( 'NONE',  ( 1.910449006669871087E-17, 0.4763888888888885287, -0.3119999999999999996 ) ) ;
#19849 = CARTESIAN_POINT ( 'NONE',  ( -0.2206173157302027676, 4.668833333333332725, 0.2206173157302028787 ) ) ;
#19850 = VECTOR ( 'NONE', #13261, 39.37007874015748143 ) ;
#19851 = ADVANCED_FACE ( 'NONE', ( #7293 ), #3623, .T. ) ;
#19852 = CARTESIAN_POINT ( 'NONE',  ( -0.2819296736111110979, 4.127166666742532186, -0.1167790944451422980 ) ) ;
#19853 = CARTESIAN_POINT ( 'NONE',  ( 0.1993543840281267465, 3.832027777853643791, 0.1993543840281266633 ) ) ;
#19854 = CARTESIAN_POINT ( 'NONE',  ( -0.4500000000000003997, 0.2598076211353315679, 0.3779506566538943790 ) ) ;
#19855 = CARTESIAN_POINT ( 'NONE',  ( 2.319244702705236527, 2.291712385858714285, -2.476240473580833878 ) ) ;
#19856 = ORIENTED_EDGE ( 'NONE', *, *, #13651, .F. ) ;
#19857 = CARTESIAN_POINT ( 'NONE',  ( 8.375559671162349491E-15, 3.988277777929486678, -0.3119999999999999996 ) ) ;
#19858 = CARTESIAN_POINT ( 'NONE',  ( 0.2819296736111110979, 4.488277777853643791, 0.1167790944451422425 ) ) ;
#19859 = ADVANCED_FACE ( 'NONE', ( #12923 ), #11195, .T. ) ;
#19860 = CARTESIAN_POINT ( 'NONE',  ( -0.3100117717788872240, 4.501197505690473832, -0.03525460809166135884 ) ) ;
#19861 = APPROVAL_ROLE ( '' ) ;
#19862 = CARTESIAN_POINT ( 'NONE',  ( 0.000000000000000000, 5.384999999999999787, -0.3119999999999999996 ) ) ;
#19863 = AXIS2_PLACEMENT_3D ( 'NONE', #8232, #3118, #15564 ) ;
#19864 = CARTESIAN_POINT ( 'NONE',  ( -0.2764156081756484196, 0.1144950937579609918, 0.08486111111111295513 ) ) ;
#19865 = ADVANCED_BREP_SHAPE_REPRESENTATION ( '', ( #17087, #9127 ), #2886 ) ;
#19866 = CIRCLE ( 'NONE', #5475, 0.3125000000000000000 ) ;
#19867 = B_SPLINE_CURVE_WITH_KNOTS ( 'NONE', 3,
 ( #11586, #236, #20837, #7902, #20717, #2311, #15354, #13543, #6077, #11339, #7672, #5839, #9872, #17185, #21076, #6195, #4013, #4366, #17299, #11703, #9626, #18894, #19015, #15122, #109, #13302, #22548, #2195, #11461, #352, #13185, #18647, #5726, #20958, #2063, #18768, #4251, #1940, #9748, #9387, #19126, #7793, #2430, #15237, #592, #22666 ),
 .UNSPECIFIED., .F., .F.,
 ( 4, 2, 2, 2, 2, 2, 2, 2, 2, 2, 2, 2, 2, 2, 2, 2, 2, 2, 2, 2, 2, 2, 4 ),
 ( 0.007005524140355982865, 0.007790685184056548099, 0.008575846227757113333, 0.01014616831515824553, 0.01093132935885880903, 0.01171649040255937427, 0.01328681248996050820, 0.01485713457736164041, 0.01564229562106220217, 0.01642745666476276914, 0.01799777875216388573, 0.01956810083956500579, 0.02113842292696612585, 0.02192358397066668935, 0.02270874501436724591, 0.02349390605806780941, 0.02427906710176836944, 0.02584938918916948949, 0.02741971127657060955, 0.02899003336397173308, 0.02977519440767229658, 0.03056035545137285314, 0.03213067753877397320 ),
 .UNSPECIFIED. ) ;
#19868 = CARTESIAN_POINT ( 'NONE',  ( -0.1993543840281266355, 4.151472222298088433, 0.1993543840281267465 ) ) ;
#19869 = CARTESIAN_POINT ( 'NONE',  ( -0.09821183740504324522, 4.824495949122511895, -0.2968094086098724271 ) ) ;
#19870 = CARTESIAN_POINT ( 'NONE',  ( 0.4500000000000003442, -0.2598076211353317344, 0.3779506566538943235 ) ) ;
#19871 = CARTESIAN_POINT ( 'NONE',  ( 0.1954553509668046640, -0.1954553509668047195, 0.1716666666666691599 ) ) ;
#19872 = CARTESIAN_POINT ( 'NONE',  ( -0.3613381517857143232, 0.04732142847388615819, -4.425116109941954795E-17 ) ) ;
#19873 = CARTESIAN_POINT ( 'NONE',  ( 0.1993543840281266910, 0.6118055554796889561, -0.1993543840281266910 ) ) ;
#19874 = CARTESIAN_POINT ( 'NONE',  ( 0.000000000000000000, 3.700000000000000622, 0.000000000000000000 ) ) ;
#19875 = CARTESIAN_POINT ( 'NONE',  ( 0.000000000000000000, 0.3308333333333335347, -0.1199999999999999956 ) ) ;
#19876 = CARTESIAN_POINT ( 'NONE',  ( 0.1954553509668046640, -0.1954553509668047195, -0.05749999999999928085 ) ) ;
#19877 = CARTESIAN_POINT ( 'NONE',  ( 0.1306872919485616846, 0.3155070326520292290, 0.4338194444444488651 ) ) ;
#19878 = ORIENTED_EDGE ( 'NONE', *, *, #3372, .F. ) ;
#19879 = ORIENTED_EDGE ( 'NONE', *, *, #13533, .F. ) ;
#19880 = CARTESIAN_POINT ( 'NONE',  ( -0.3999999999999999667, 0.07499999999999995559, -0.1299678784931626030 ) ) ;
#19881 =( BOUNDED_CURVE ( )  B_SPLINE_CURVE ( 2, ( #3320, #19669, #10777, #18203, #1499, #21382, #2840, #1017, #8447 ),
 .UNSPECIFIED., .F., .F. ) 
 B_SPLINE_CURVE_WITH_KNOTS ( ( 3, 2, 2, 2, 3 ),
 ( 0.4910714285714283811, 0.4955357142857142461, 0.5000000000000000000, 0.5044642857142858094, 0.5089285714285716189 ),
 .UNSPECIFIED. ) 
 CURVE ( )  GEOMETRIC_REPRESENTATION_ITEM ( )  RATIONAL_B_SPLINE_CURVE ( ( 1.000000000000002887, 0.9238795325112838519, 1.000000000000000000, 0.9238795325112867385, 1.000000000000000000, 0.9238795325112867385, 1.000000000000000000, 0.9238795325112829637, 1.000000000000003775 ) ) 
 REPRESENTATION_ITEM ( '' )  );
#19882 = CARTESIAN_POINT ( 'NONE',  ( 0.4687500000000002220, 0.1778880616680548199, 0.4111843359142061671 ) ) ;
#19883 = CARTESIAN_POINT ( 'NONE',  ( 0.2819296736111110979, 0.4243055554796889006, 0.000000000000000000 ) ) ;
#19884 = ADVANCED_FACE ( 'NONE', ( #3873 ), #18624, .T. ) ;
#19885 = CARTESIAN_POINT ( 'NONE',  ( 0.1993543840281267465, 3.832027777853643791, 0.1993543840281266633 ) ) ;
#19886 = CARTESIAN_POINT ( 'NONE',  ( 0.2923287055106771337, 0.01874999990245761194, -0.2123892367102620249 ) ) ;
#19887 = ORIENTED_EDGE ( 'NONE', *, *, #16922, .F. ) ;
#19888 = CARTESIAN_POINT ( 'NONE',  ( 0.1167790944451424368, 4.439666666742532186, 0.2819296736111110424 ) ) ;
#19889 = CARTESIAN_POINT ( 'NONE',  ( 0.2026171589331097200, 5.137660913757319037, -0.2291522707572892226 ) ) ;
#19890 = DIRECTION ( 'NONE',  ( -0.000000000000000000, 1.000000000000000000, -0.000000000000000000 ) ) ;
#19891 = AXIS2_PLACEMENT_3D ( 'NONE', #10658, #23679, #23801 ) ;
#19892 = VERTEX_POINT ( 'NONE', #3505 ) ;
#19893 = CARTESIAN_POINT ( 'NONE',  ( 0.1292346314604009005, 4.012583333333331836, 0.3120000000000048845 ) ) ;
#19894 = CARTESIAN_POINT ( 'NONE',  ( -0.3119999999999998885, 3.727861111262843252, 0.1292346314604058410 ) ) ;
#19895 = ADVANCED_FACE ( 'NONE', ( #11073 ), #23850, .F. ) ;
#19896 = CARTESIAN_POINT ( 'NONE',  ( 0.2604525334828327598, 4.191421240092715550, 0.1717991962690550156 ) ) ;
#19897 = B_SPLINE_CURVE_WITH_KNOTS ( 'NONE', 3,
 ( #1944, #5729, #5362, #24011, #20364, #13188, #9390, #24124, #20247, #12828, #1707, #9144, #16707, #7321, #16941, #20602, #7439, #12952, #240, #7675, #18898, #15125, #22551, #16589, #14772, #22187, #11466, #5487, #3655, #1822, #19129, #21200, #8028, #4132, #6200, #2551, #23020, #11957, #12074, #2781, #20961, #17424, #17544, #22786, #2433, #9751, #6440 ),
 .UNSPECIFIED., .F., .F.,
 ( 4, 2, 2, 2, 2, 2, 2, 2, 2, 2, 2, 2, 2, 2, 2, 2, 2, 2, 2, 2, 2, 1, 2, 4 ),
 ( 0.01742734353126568214, 0.01820292306817463193, 0.01897850260508358519, 0.02052966167890148130, 0.02208082075271938088, 0.02285640028962833067, 0.02363197982653728046, 0.02518313890035518005, 0.02673429797417307963, 0.02828545704799098268, 0.02906103658489993247, 0.02983661612180887879, 0.03138777519562677837, 0.03293893426944467795, 0.03371451380635362427, 0.03449009334326257059, 0.03604125241708047711, 0.03681683195398942343, 0.03759241149089836975, 0.03914357056471626933, 0.03991915010162521565, 0.04069472963853416891, 0.04147030917544311523, 0.04224588871235206156 ),
 .UNSPECIFIED. ) ;
#19898 = CARTESIAN_POINT ( 'NONE',  ( -9.626299801968715084E-16, 0.2660714283763437327, -0.4000000000000000222 ) ) ;
#19899 = CARTESIAN_POINT ( 'NONE',  ( -0.1993543840281266355, 4.970916666742532186, 0.1993543840281267465 ) ) ;
#19900 = PERSON_AND_ORGANIZATION ( #23967, #1018 ) ;
#19901 = ORIENTED_EDGE ( 'NONE', *, *, #8392, .F. ) ;
#19902 = CARTESIAN_POINT ( 'NONE',  ( -0.3119999999999999996, 0.3166666665149337478, -3.820898013339742174E-17 ) ) ;
#19903 = EDGE_CURVE ( 'NONE', #18582, #23659, #10320, .T. ) ;
#19904 = CARTESIAN_POINT ( 'NONE',  ( -0.1292346314604056190, 0.1951388887371559577, -0.3119999999999999996 ) ) ;
#19905 = EDGE_LOOP ( 'NONE', ( #14576, #14754, #16587, #13504 ) ) ;
#19906 = CARTESIAN_POINT ( 'NONE',  ( 0.1993543840281266355, 0.3201388888130222710, 0.1993543840281267465 ) ) ;
#19907 = CIRCLE ( 'NONE', #14473, 0.4624999999999992450 ) ;
#19908 = VERTEX_POINT ( 'NONE', #5935 ) ;
#19909 = CARTESIAN_POINT ( 'NONE',  ( 0.4449999999999992295, 0.000000000000000000, -0.04999999999999918399 ) ) ;
#19910 = CARTESIAN_POINT ( 'NONE',  ( 0.3125000000000000000, -5.740531871003217465E-17, 0.3175000000000038347 ) ) ;
#19911 = CARTESIAN_POINT ( 'NONE',  ( -0.5116234456863466562, 0.7841300617983539833, 2.549370209580444691 ) ) ;
#19912 = CARTESIAN_POINT ( 'NONE',  ( -0.1236067977499790416, 0.02142857142857140795, 0.3804226065180614236 ) ) ;
#19913 = CARTESIAN_POINT ( 'NONE',  ( -0.03602220318626091905, 5.044808164693691310, -0.3105944775966490434 ) ) ;
#19914 = CARTESIAN_POINT ( 'NONE',  ( 0.3120000000000000551, 4.186194444444444329, 0.1292346314604056190 ) ) ;
#19915 = EDGE_CURVE ( 'NONE', #19560, #8097, #6054, .T. ) ;
#19916 = CARTESIAN_POINT ( 'NONE',  ( -0.2703837395707749391, 3.895695782031614929, 0.1575116891411247888 ) ) ;
#19917 = CARTESIAN_POINT ( 'NONE',  ( 0.5997114317030027841, 2.291712385858714729, -1.145928253224826276 ) ) ;
#19918 = EDGE_CURVE ( 'NONE', #6853, #19892, #11928, .T. ) ;
#19919 = EDGE_CURVE ( 'NONE', #7279, #21116, #21917, .T. ) ;
#19920 = CARTESIAN_POINT ( 'NONE',  ( 0.1993543840281267465, 4.609805555631421470, 0.1993543840281266633 ) ) ;
#19921 = DIRECTION ( 'NONE',  ( -1.000000000000000000, 0.000000000000000000, 0.000000000000000000 ) ) ;
#19922 = CARTESIAN_POINT ( 'NONE',  ( 0.2819296736111110424, 3.828555555631421026, -0.1167790944451423396 ) ) ;
#19923 = CARTESIAN_POINT ( 'NONE',  ( 1.779986855112097865, 2.978485840173427324, -2.386288568296997870 ) ) ;
#19924 = LINE ( 'NONE', #8453, #5166 ) ;
#19925 = CARTESIAN_POINT ( 'NONE',  ( 0.09085534873164523295, 5.072999999999999510, 0.3012414626474842483 ) ) ;
#19926 = CARTESIAN_POINT ( 'NONE',  ( -0.05310794838523746897, 4.792355782325940616, 0.3074473702546657305 ) ) ;
#19927 = CARTESIAN_POINT ( 'NONE',  ( 5.731347020009612645E-17, 4.349388889040620931, 0.3119999999999999996 ) ) ;
#19928 = EDGE_CURVE ( 'NONE', #2118, #12608, #568, .T. ) ;
#19929 = CARTESIAN_POINT ( 'NONE',  ( -0.1993543840281266355, 4.651472222298087544, 0.1993543840281267465 ) ) ;
#19930 = B_SPLINE_CURVE_WITH_KNOTS ( 'NONE', 3,
 ( #8874, #3029, #12313, #10711, #14009, #19726, #18022, #19488, #3260, #23130, #17906, #10594, #19605, #21682, #15947, #4613, #1201, #16077, #6805, #12432, #6442, #13895, #23373, #14246, #1319, #23249, #2900, #949, #12075, #12198, #4726, #4965, #8744, #10358, #16199, #17782, #16681, #7413, #7171 ),
 .UNSPECIFIED., .F., .F.,
 ( 4, 2, 1, 1, 1, 1, 1, 2, 2, 2, 2, 2, 2, 2, 2, 2, 2, 2, 2, 2, 2, 4 ),
 ( 0.6122134677491346544, 0.6122179294325030829, 0.6122223911158716225, 0.6122313144826084796, 0.6122491612160823049, 0.6122848546830299554, 0.6123562416169253675, 0.6124990154847160806, 0.6127845632202973958, 0.6133556586914602482, 0.6144978496337858420, 0.6156400405761114358, 0.6167822315184370296, 0.6179244224607626235, 0.6190666134030882173, 0.6202088043454138111, 0.6213509952877394049, 0.6224931862300648877, 0.6236353771723904815, 0.6259197590570416692, 0.6282041409416928568, 0.6304885228263440444 ),
 .UNSPECIFIED. ) ;
#19931 = CARTESIAN_POINT ( 'NONE',  ( 0.1993543840281266633, 3.776472222298087988, -0.1993543840281266910 ) ) ;
#19932 = ORIENTED_EDGE ( 'NONE', *, *, #18817, .F. ) ;
#19933 = ORIENTED_EDGE ( 'NONE', *, *, #23301, .F. ) ;
#19934 = DATE_AND_TIME ( #23936, #23178 ) ;
#19935 = CARTESIAN_POINT ( 'NONE',  ( 0.4449999999999992295, 0.000000000000000000, -0.04999999999999918399 ) ) ;
#19936 = DIRECTION ( 'NONE',  ( -0.8660254037844434816, -0.000000000000000000, -0.4999999999999914513 ) ) ;
#19937 = VERTEX_POINT ( 'NONE', #13393 ) ;
#19938 = CARTESIAN_POINT ( 'NONE',  ( -0.2206173157302028787, 0.2680555554038226429, 0.2206173157302027954 ) ) ;
#19939 = CARTESIAN_POINT ( 'NONE',  ( -0.02010730444239897108, 4.377710753833683910, -0.3113796951532629143 ) ) ;
#19940 = CARTESIAN_POINT ( 'NONE',  ( -0.2094265943819361708, 3.717041492013063220, -0.2313614939596641551 ) ) ;
#19941 = CARTESIAN_POINT ( 'NONE',  ( -1.858121103377620624E-07, 4.877166671810766019, -0.3119999999999446549 ) ) ;
#19942 = CARTESIAN_POINT ( 'NONE',  ( 0.2102303072135171258, 0.3429911158895919132, -0.7199368671688829435 ) ) ;
#19943 = ORIENTED_EDGE ( 'NONE', *, *, #17829, .T. ) ;
#19944 = ORIENTED_EDGE ( 'NONE', *, *, #2636, .F. ) ;
#19945 = CARTESIAN_POINT ( 'NONE',  ( 0.000000000000000000, 0.000000000000000000, 0.000000000000000000 ) ) ;
#19946 = CARTESIAN_POINT ( 'NONE',  ( 0.2819296736111110979, 0.2611111110352444808, -0.1167790944451422980 ) ) ;
#19947 = CARTESIAN_POINT ( 'NONE',  ( -0.2764156081756484196, -0.1144950937579609362, 0.3695833333333374826 ) ) ;
#19948 = CARTESIAN_POINT ( 'NONE',  ( -0.2819296736111110424, 4.411888888964753619, 0.1167790944451424923 ) ) ;
#19949 = CARTESIAN_POINT ( 'NONE',  ( 0.3119999999999999996, 0.1847222222222218990, 0.000000000000000000 ) ) ;
#19950 = LINE ( 'NONE', #4704, #16453 ) ;
#19951 = CARTESIAN_POINT ( 'NONE',  ( -0.02037115866045762641, 4.237742989552504724, 0.3115008212664499010 ) ) ;
#19952 = CARTESIAN_POINT ( 'NONE',  ( -0.2206173157302028232, 3.988277777777776922, -0.2206173157302028232 ) ) ;
#19953 = EDGE_CURVE ( 'NONE', #12009, #16668, #16469, .T. ) ;
#19954 = CARTESIAN_POINT ( 'NONE',  ( -0.1292346314604056745, 4.991750000151732536, -0.3119999999999999996 ) ) ;
#19955 = CIRCLE ( 'NONE', #21510, 0.1850000000000000533 ) ;
#19956 = EDGE_CURVE ( 'NONE', #21724, #18346, #17399, .T. ) ;
#19957 = ORIENTED_EDGE ( 'NONE', *, *, #10816, .F. ) ;
#19958 = CYLINDRICAL_SURFACE ( 'NONE', #1565, 0.3125000000000000000 ) ;
#19959 = ORIENTED_EDGE ( 'NONE', *, *, #23884, .F. ) ;
#19960 = FACE_OUTER_BOUND ( 'NONE', #21167, .T. ) ;
#19961 = CARTESIAN_POINT ( 'NONE',  ( -0.2230971623002953874, 0.2230971623002954152, 0.3365972222222262666 ) ) ;
#19962 = CARTESIAN_POINT ( 'NONE',  ( -0.3613381517857143232, 0.3330357141881718497, -4.425116109941954795E-17 ) ) ;
#19963 = CIRCLE ( 'NONE', #13347, 0.7500000000000001110 ) ;
#19964 = CARTESIAN_POINT ( 'NONE',  ( 0.4212185919419055291, -0.2861805174101255678, 0.4063787963957714577 ) ) ;
#19965 = CARTESIAN_POINT ( 'NONE',  ( 0.2923287055106771337, 0.2008928570453147044, 0.2123892367102621359 ) ) ;
#19966 = CARTESIAN_POINT ( 'NONE',  ( -0.2819296736111110979, 0.2993055554796889561, -3.452642723725051716E-17 ) ) ;
#19967 = CARTESIAN_POINT ( 'NONE',  ( -3.385114897866767815E-17, -0.2764156081756484196, 0.1091666666666686880 ) ) ;
#19968 = CARTESIAN_POINT ( 'NONE',  ( 0.1167790944451422702, 5.238277777853643791, -0.2819296736111110424 ) ) ;
#19969 = CARTESIAN_POINT ( 'NONE',  ( 0.3049278984963029182, 4.472535498897220130, 0.06605302570197388312 ) ) ;
#19970 = VERTEX_POINT ( 'NONE', #15691 ) ;
#19971 = CARTESIAN_POINT ( 'NONE',  ( -0.1539092610705375952, 4.603981316102501609, -0.2721373798033744906 ) ) ;
#19972 = APPROVAL ( #1215, 'UNSPECIFIED' ) ;
#19973 = DIRECTION ( 'NONE',  ( 0.000000000000000000, 0.000000000000000000, 1.000000000000000000 ) ) ;
#19974 = CARTESIAN_POINT ( 'NONE',  ( 0.3613381517857143232, 0.4223214284738860957, 0.000000000000000000 ) ) ;
#19975 = CARTESIAN_POINT ( 'NONE',  ( 0.1292346314604057300, 0.5562499998482671737, 0.3119999999999998885 ) ) ;
#19976 = CARTESIAN_POINT ( 'NONE',  ( -0.3119999999999999996, 4.717444444444443441, 0.000000000000000000 ) ) ;
#19977 = CARTESIAN_POINT ( 'NONE',  ( 0.2819296736111111534, 4.099388888964754507, 0.1167790944451422563 ) ) ;
#19978 = CARTESIAN_POINT ( 'NONE',  ( 9.184850993605150903E-17, 2.735000000000000320, -0.7500000000000001110 ) ) ;
#19979 = DIRECTION ( 'NONE',  ( 0.000000000000000000, 1.000000000000000000, 0.000000000000000000 ) ) ;
#19980 = CARTESIAN_POINT ( 'NONE',  ( 1.910449006669871087E-17, 0.5249999998482670627, -0.3119999999999999996 ) ) ;
#19981 = ORIENTED_EDGE ( 'NONE', *, *, #59, .T. ) ;
#19982 = CARTESIAN_POINT ( 'NONE',  ( -0.3125000000000000000, -0.1294417382415921913, 0.1195833333333352622 ) ) ;
#19983 = CARTESIAN_POINT ( 'NONE',  ( 0.1167790944451424368, 4.481333333409199149, 0.2819296736111110424 ) ) ;
#19984 = AXIS2_PLACEMENT_3D ( 'NONE', #1863, #9062, #14442 ) ;
#19985 = CARTESIAN_POINT ( 'NONE',  ( -0.2371201309373563992, 4.508458841826880281, 0.2028076677489544510 ) ) ;
#19986 = SHAPE_DEFINITION_REPRESENTATION ( #12666, #12001 ) ;
#19987 = CARTESIAN_POINT ( 'NONE',  ( -0.4687500000000016098, -0.2629282712287717705, 0.05975564523638846742 ) ) ;
#19988 = CARTESIAN_POINT ( 'NONE',  ( 0.1954553509668046640, -0.1954553509668047195, 0.2202777777777807366 ) ) ;
#19989 = CARTESIAN_POINT ( 'NONE',  ( 5.178964085587577574E-17, 4.102861111186976828, 0.2819296736111110979 ) ) ;
#19990 = EDGE_CURVE ( 'NONE', #8463, #5917, #6509, .T. ) ;
#19991 = CARTESIAN_POINT ( 'NONE',  ( -0.3109883961989257095, 4.834813968162577247, -0.02511538183358531101 ) ) ;
#19992 = CARTESIAN_POINT ( 'NONE',  ( -0.02037388374998021570, 4.433306081093942197, -0.3120000000000003326 ) ) ;
#19993 = CARTESIAN_POINT ( 'NONE',  ( -0.1144950937579609779, 0.2764156081756484196, 0.3626388888888929518 ) ) ;
#19994 = CARTESIAN_POINT ( 'NONE',  ( 0.1116596296178199027, 0.06874999990245758696, 0.3436530038418508792 ) ) ;
#19995 = CARTESIAN_POINT ( 'NONE',  ( -0.1993543840281266633, 0.5701388888130222155, -0.1993543840281266910 ) ) ;
#19996 = CARTESIAN_POINT ( 'NONE',  ( 0.4687500000000003886, 0.08694521043083575096, 0.07655001303618025332 ) ) ;
#19997 = CARTESIAN_POINT ( 'NONE',  ( 1.573500000000000343, 2.683750000000000746, -1.006250000000000533 ) ) ;
#19998 = APPROVAL ( #23038, 'UNKNOWN' ) ;
#19999 = CARTESIAN_POINT ( 'NONE',  ( -0.1701069292077561357, 0.2394183616649627200, -0.7304681109799713301 ) ) ;
#20000 = CARTESIAN_POINT ( 'NONE',  ( 0.2764156081756484196, -5.077672346800151106E-17, 0.06055555555555720143 ) ) ;
#20001 = CARTESIAN_POINT ( 'NONE',  ( -0.3155070326520292845, 1.931923388228935888E-17, 0.4511805555555600811 ) ) ;
#20002 = VECTOR ( 'NONE', #10753, 39.37007874015748854 ) ;
#20003 = VERTEX_POINT ( 'NONE', #19701 ) ;
#20004 = ORIENTED_EDGE ( 'NONE', *, *, #5591, .T. ) ;
#20005 = CARTESIAN_POINT ( 'NONE',  ( 0.1649704474213681549, 0.4586382700592834261, 0.07155713030921630191 ) ) ;
#20006 = CARTESIAN_POINT ( 'NONE',  ( 0.1167790944451423119, 0.6013888888130222155, -0.2819296736111110979 ) ) ;
#20007 = CARTESIAN_POINT ( 'NONE',  ( -0.1993543840281267465, 0.5701388888130222155, 0.1993543840281266633 ) ) ;
#20008 = CARTESIAN_POINT ( 'NONE',  ( 5.178964085587577574E-17, 3.769527777853644235, 0.2819296736111110979 ) ) ;
#20009 = CARTESIAN_POINT ( 'NONE',  ( 2.326421213736078119E-17, 0.1008928570453146989, -0.3799334167787516425 ) ) ;
#20010 = CARTESIAN_POINT ( 'NONE',  ( -0.1993543840281266355, 4.318138888964754507, 0.1993543840281267465 ) ) ;
#20011 = CARTESIAN_POINT ( 'NONE',  ( 1.522235971340160240E-16, 0.1799999999999999933, 1.243000000000000105 ) ) ;
#20012 = CARTESIAN_POINT ( 'NONE',  ( -0.3119999999999999996, 4.384111111111110404, 0.000000000000000000 ) ) ;
#20013 = ORIENTED_EDGE ( 'NONE', *, *, #16842, .F. ) ;
#20014 = CARTESIAN_POINT ( 'NONE',  ( 0.3090122127097978399, 4.364796073349109129, -0.05326403159567110607 ) ) ;
#20015 = CARTESIAN_POINT ( 'NONE',  ( 0.1993543840281266633, 5.220916666742532186, -0.1993543840281266910 ) ) ;
#20016 = CARTESIAN_POINT ( 'NONE',  ( 0.2252836021529972255, 4.203383026810429079, -0.2159527458307812231 ) ) ;
#20017 = AXIS2_PLACEMENT_3D ( 'NONE', #8145, #6321, #19487 ) ;
#20018 = CARTESIAN_POINT ( 'NONE',  ( -1.726321361862525858E-17, 4.838972222298088433, -0.2819296736111110979 ) ) ;
#20020 = ADVANCED_FACE ( 'NONE', ( #17757 ), #23706, .T. ) ;
#20019 = PERSON_AND_ORGANIZATION_ROLE ( 'classification_officer' ) ;
#20021 = ORIENTED_EDGE ( 'NONE', *, *, #21130, .F. ) ;
#20022 = CARTESIAN_POINT ( 'NONE',  ( 0.000000000000000000, 3.700000000000000622, -0.4000000000000000222 ) ) ;
#20023 = CARTESIAN_POINT ( 'NONE',  ( 0.4749999999999999778, 3.575000000000000622, -0.09499999999999995948 ) ) ;
#20024 = ORIENTED_EDGE ( 'NONE', *, *, #9760, .T. ) ;
#20025 = CARTESIAN_POINT ( 'NONE',  ( -5.178964085587577574E-17, 0.2020833332574667185, 0.2819296736111110979 ) ) ;
#20026 = ORIENTED_EDGE ( 'NONE', *, *, #12902, .F. ) ;
#20027 = CARTESIAN_POINT ( 'NONE',  ( 0.3003475124358242487, 3.066692553488282957, 3.638968604327563749 ) ) ;
#20028 = DIRECTION ( 'NONE',  ( 0.000000000000000000, -0.7071067811865459074, -0.7071067811865492381 ) ) ;
#20029 = CARTESIAN_POINT ( 'NONE',  ( -0.4516234456863466584, 0.4427737985694512046, 2.584011225731822403 ) ) ;
#20030 = CARTESIAN_POINT ( 'NONE',  ( -0.3236067977499789694, -0.07142857142857143848, -0.2351141009169893104 ) ) ;
#20031 = EDGE_CURVE ( 'NONE', #7205, #18597, #12279, .T. ) ;
#20032 = DIRECTION ( 'NONE',  ( -0.4472135954999558738, -0.4472135954999557628, -0.7745966692414858468 ) ) ;
#20033 = CARTESIAN_POINT ( 'NONE',  ( -0.2933312968388447906, 3.887856832897826909, -0.1097277311388216714 ) ) ;
#20034 = DIRECTION ( 'NONE',  ( -0.4999999999999760192, 0.000000000000000000, 0.8660254037844524744 ) ) ;
#20035 = CARTESIAN_POINT ( 'NONE',  ( 0.1167790944451422702, 4.404944444520309865, -0.2819296736111110424 ) ) ;
#20036 = DIRECTION ( 'NONE',  ( 0.000000000000000000, 1.000000000000000000, 0.000000000000000000 ) ) ;
#20037 = CARTESIAN_POINT ( 'NONE',  ( -0.3119999999999999996, 0.2576388887371560132, -0.1292346314604056745 ) ) ;
#20038 = AXIS2_PLACEMENT_3D ( 'NONE', #19413, #4416, #6244 ) ;
#20039 = CARTESIAN_POINT ( 'NONE',  ( -0.2819296736111110424, 5.141055555631421470, -0.1167790944451423119 ) ) ;
#20040 = CARTESIAN_POINT ( 'NONE',  ( -0.2909984631779261588, 0.05351298515340481565, 0.08506003772084960723 ) ) ;
#20041 = CARTESIAN_POINT ( 'NONE',  ( 0.3071603949907269482, 3.750640993411230362, 0.05477998771989885801 ) ) ;
#20042 = DIRECTION ( 'NONE',  ( -0.000000000000000000, -1.000000000000000000, -0.000000000000000000 ) ) ;
#20043 = CARTESIAN_POINT ( 'NONE',  ( -0.1236067977499790416, 0.2267857140906294755, 0.3804226065180614236 ) ) ;
#20044 = CARTESIAN_POINT ( 'NONE',  ( -0.1292346314604056745, 4.325083333485065573, -0.3119999999999999996 ) ) ;
#20045 = CARTESIAN_POINT ( 'NONE',  ( 0.2819296736111110979, 4.509111111186976828, -0.1167790944451423396 ) ) ;
#20046 = CARTESIAN_POINT ( 'NONE',  ( 5.178964085587577574E-17, 3.922305555631421026, 0.2819296736111110979 ) ) ;
#20047 =( BOUNDED_CURVE ( )  B_SPLINE_CURVE ( 2, ( #19600, #23015, #13769, #21195, #4486, #19367, #3842, #16531, #9209, #174, #9449, #9082, #5425, #20424, #3721, #24071, #16651, #1766, #14712, #22125, #2013, #14831, #7379, #11167, #18596, #51, #14943, #11043, #16768, #18715, #22247, #13131, #11284, #7616, #16883, #12892, #18473, #5545, #20662, #15067, #7735, #1887, #15180, #3959, #11402, #13247, #297, #13009, #22365, #9329, #3474, #7498, #5668, #20546, #22489, #5785, #23950, #9570, #7264, #18834, #20307, #2130, #17002, #4961, #10925, #12428, #20186, #18355, #1647, #3592, #13833, #6139, #20902, #17250, #13487, #9692, #10059, #6263, #8327, #23076, #5902, #534, #15422, #4431, #419, #13605, #11527, #4195, #17130, #13722, #8086, #896, #13361, #7971, #4556, #2729, #4072, #22617, #15537, #22961, #2381, #6018, #21143, #11898, #12018, #17605, #21020, #2258, #20781, #7852, #4313, #6384, #17483, #19430, #22849, #19315, #15301, #11768, #21266, #2616, #18959, #777, #10182, #22730, #11649 ),
 .UNSPECIFIED., .F., .F. ) 
 B_SPLINE_CURVE_WITH_KNOTS ( ( 3, 2, 2, 2, 2, 2, 2, 2, 2, 2, 2, 2, 2, 2, 2, 2, 2, 2, 2, 2, 2, 2, 2, 2, 2, 2, 2, 2, 2, 2, 2, 2, 2, 2, 2, 2, 2, 2, 2, 2, 2, 2, 2, 2, 2, 2, 2, 2, 2, 2, 2, 2, 2, 2, 2, 2, 2, 2, 2, 2, 2, 2, 3 ),
 ( 0.1196839499064063089, 0.1285714285714285587, 0.1428571428571428492, 0.1571428571428571397, 0.1714285714285714302, 0.1857142857142857206, 0.2000000000000000111, 0.2142857142857142738, 0.2285714285714285643, 0.2428571428571428825, 0.2571428571428571175, 0.2714285714285714080, 0.2857142857142856984, 0.2999999999999999889, 0.3142857142857142794, 0.3285714285714285698, 0.3428571428571428603, 0.3571428571428571508, 0.3714285714285714413, 0.3857142857142857317, 0.4000000000000000222, 0.4142857142857143127, 0.4285714285714285476, 0.4428571428571428381, 0.4571428571428571286, 0.4714285714285714191, 0.4857142857142857095, 0.4999999999999999445, 0.5142857142857142350, 0.5285714285714285809, 0.5428571428571428159, 0.5571428571428571619, 0.5714285714285713969, 0.5857142857142857428, 0.5999999999999999778, 0.6142857142857143238, 0.6285714285714285587, 0.6428571428571429047, 0.6571428571428571397, 0.6714285714285713746, 0.6857142857142857206, 0.6999999999999999556, 0.7142857142857143016, 0.7285714285714285365, 0.7428571428571428825, 0.7571428571428571175, 0.7714285714285714635, 0.7857142857142856984, 0.8000000000000000444, 0.8142857142857142794, 0.8285714285714286254, 0.8428571428571428603, 0.8571428571428570953, 0.8714285714285714413, 0.8857142857142857872, 0.9000000000000000222, 0.9142857142857142572, 0.9285714285714286031, 0.9428571428571428381, 0.9571428571428571841, 0.9714285714285715301, 0.9857142857142857650, 1.000000000000000000 ),
 .UNSPECIFIED. ) 
 CURVE ( )  GEOMETRIC_REPRESENTATION_ITEM ( )  RATIONAL_B_SPLINE_CURVE ( ( 0.9769881591460136683, 0.9695511082946919323, 1.000000000000000000, 0.9510565162951535312, 1.000000000000000000, 0.9510565162951535312, 1.000000000000000000, 0.9510565162951535312, 1.000000000000000000, 0.9510565162951535312, 1.000000000000000000, 0.9510565162951535312, 1.000000000000000000, 0.9510565162951535312, 1.000000000000000000, 0.9510565162951535312, 1.000000000000000000, 0.9510565162951535312, 1.000000000000000000, 0.9510565162951535312, 1.000000000000000000, 0.9510565162951535312, 1.000000000000000000, 0.9510565162951535312, 1.000000000000000000, 0.9510565162951535312, 1.000000000000000000, 0.9510565162951535312, 1.000000000000000000, 0.9510565162951535312, 1.000000000000000000, 0.9510565162951535312, 1.000000000000000000, 0.9510565162951535312, 1.000000000000000000, 0.9510565162951535312, 1.000000000000000000, 0.9510565162951535312, 1.000000000000000000, 0.9510565162951535312, 1.000000000000000000, 0.9510565162951535312, 1.000000000000000000, 0.9510565162951535312, 1.000000000000000000, 0.9510565162951535312, 1.000000000000000000, 0.9510565162951535312, 1.000000000000000000, 0.9510565162951535312, 1.000000000000000000, 0.9510565162951535312, 1.000000000000000000, 0.9510565162951535312, 1.000000000000000000, 0.9510565162951535312, 1.000000000000000000, 0.9510565162951535312, 1.000000000000000000, 0.9510565162951535312, 1.000000000000000000, 0.9510565162951535312, 1.000000000000000000, 0.9510565162951535312, 1.000000000000000000, 0.9510565162951535312, 1.000000000000000000, 0.9510565162951535312, 1.000000000000000000, 0.9510565162951535312, 1.000000000000000000, 0.9510565162951535312, 1.000000000000000000, 0.9510565162951535312, 1.000000000000000000, 0.9510565162951535312, 1.000000000000000000, 0.9510565162951535312, 1.000000000000000000, 0.9510565162951535312, 1.000000000000000000, 0.9510565162951535312, 1.000000000000000000, 0.9510565162951535312, 1.000000000000000000, 0.9510565162951535312, 1.000000000000000000, 0.9510565162951535312, 1.000000000000000000, 0.9510565162951535312, 1.000000000000000000, 0.9510565162951535312, 1.000000000000000000, 0.9510565162951535312, 1.000000000000000000, 0.9510565162951535312, 1.000000000000000000, 0.9510565162951535312, 1.000000000000000000, 0.9510565162951535312, 1.000000000000000000, 0.9510565162951535312, 1.000000000000000000, 0.9510565162951535312, 1.000000000000000000, 0.9510565162951535312, 1.000000000000000000, 0.9510565162951535312, 1.000000000000000000, 0.9510565162951535312, 1.000000000000000000, 0.9510565162951535312, 1.000000000000000000, 0.9510565162951535312, 1.000000000000000000, 0.9510565162951535312, 1.000000000000000000, 0.9510565162951535312, 1.000000000000000000, 0.9510565162951535312, 1.000000000000000000, 0.9510565162951535312, 1.000000000000000000, 0.9510565162951535312, 1.000000000000000000 ) ) 
 REPRESENTATION_ITEM ( '' )  );
#20048 = ORIENTED_EDGE ( 'NONE', *, *, #14238, .T. ) ;
#20049 = EDGE_CURVE ( 'NONE', #16613, #7560, #14771, .T. ) ;
#20050 = ADVANCED_FACE ( 'NONE', ( #3004 ), #925, .T. ) ;
#20051 = EDGE_CURVE ( 'NONE', #22245, #14830, #12966, .T. ) ;
#20052 = VERTEX_POINT ( 'NONE', #20821 ) ;
#20053 = CALENDAR_DATE ( 2026, 7, 10 ) ;
#20054 = AXIS2_PLACEMENT_3D ( 'NONE', #6521, #913, #17742 ) ;
#20055 = CARTESIAN_POINT ( 'NONE',  ( 7.699581739047377146E-15, 4.099388889040679551, -0.3119999999999999996 ) ) ;
#20056 = DIRECTION ( 'NONE',  ( 0.000000000000000000, 0.000000000000000000, -1.000000000000000000 ) ) ;
#20057 = ORIENTED_EDGE ( 'NONE', *, *, #13785, .T. ) ;
#20058 = CARTESIAN_POINT ( 'NONE',  ( 0.3119999999999998885, 0.3409722220704892726, 0.1292346314604058410 ) ) ;
#20059 = DIRECTION ( 'NONE',  ( -0.4999999999999916733, -6.654928120984804281E-16, -0.8660254037844433705 ) ) ;
#20060 = CARTESIAN_POINT ( 'NONE',  ( -0.1410631782541221235, 3.714607375173814230, -0.2794366395611496690 ) ) ;
#20061 = DIRECTION ( 'NONE',  ( 0.08715574274765830465, -0.9961946980917454342, -3.870492493070289564E-17 ) ) ;
#20062 = CARTESIAN_POINT ( 'NONE',  ( 0.05604628919722569325, 0.1624317956547894071, -0.7480325013175007642 ) ) ;
#20063 = EDGE_CURVE ( 'NONE', #13477, #13733, #16822, .T. ) ;
#20064 = ORIENTED_EDGE ( 'NONE', *, *, #2471, .F. ) ;
#20065 = ORIENTED_EDGE ( 'NONE', *, *, #5119, .F. ) ;
#20066 = APPROVAL_PERSON_ORGANIZATION ( #23450, #16697, #2745 ) ;
#20067 = ORIENTED_EDGE ( 'NONE', *, *, #21540, .T. ) ;
#20068 = CARTESIAN_POINT ( 'NONE',  ( 2.123323208613025592, 2.690104987760001620, -2.954157130710096002 ) ) ;
#20069 = CARTESIAN_POINT ( 'NONE',  ( 0.2764156081756484196, -5.077672346800151106E-17, 0.3938888888888931739 ) ) ;
#20070 = CARTESIAN_POINT ( 'NONE',  ( 0.2819296736111110979, 4.158416666742532186, -3.452642723725051716E-17 ) ) ;
#20071 = CARTESIAN_POINT ( 'NONE',  ( -0.2819296736111110979, 5.019527777853642903, 0.000000000000000000 ) ) ;
#20072 = CARTESIAN_POINT ( 'NONE',  ( 0.000000000000000000, 5.384999999999999787, -0.3119999999999999996 ) ) ;
#20073 = LINE ( 'NONE', #16657, #7308 ) ;
#20074 = CARTESIAN_POINT ( 'NONE',  ( -0.3119999999999999996, 3.995222222222221120, 0.000000000000000000 ) ) ;
#20075 = CARTESIAN_POINT ( 'NONE',  ( 5.731347020009612645E-17, 5.016055555707287894, 0.3119999999999999996 ) ) ;
#20076 = VECTOR ( 'NONE', #5950, 39.37007874015748143 ) ;
#20077 = FACE_OUTER_BOUND ( 'NONE', #16004, .T. ) ;
#20078 = CC_DESIGN_APPROVAL ( #16697, ( #8791 ) ) ;
#20079 = CARTESIAN_POINT ( 'NONE',  ( 0.03900027537438015973, 4.683786655857547387, 0.3095907352979412885 ) ) ;
#20080 = CARTESIAN_POINT ( 'NONE',  ( -3.863846776457871776E-17, -0.3155070326520292845, 0.1907638888888917861 ) ) ;
#20081 = DIRECTION ( 'NONE',  ( -0.000000000000000000, -1.000000000000000000, -0.000000000000000000 ) ) ;
#20082 = CLOSED_SHELL ( 'NONE', ( #16148, #509, #16486, #265, #21654, #17827, #11228, #5601, #12375, #21175, #21250, #4008, #10518, #21968, #15883, #5834, #7593, #5894, #19895, #11672, #4823, #9939, #17798, #12588, #6496, #18566, #910, #6030, #23742, #4242, #4544, #4685, #20769, #5305, #18331, #20493, #9379, #3791, #9125, #20925, #15375, #3367, #16144, #6722, #7721, #2602, #8019, #15733, #6782, #1689, #4144, #5703, #10014, #9737, #17224, #4655, #20994, #12310, #16428, #12127, #21529, #19018, #13053, #4890, #21431, #6780, #7695, #10487, #12470, #5889, #10135, #10348, #2162, #17078, #7196, #21236, #8427, #23207, #8321, #23075, #4387, #7400, #22412, #17489, #24117 ) ) ;
#20083 = ORIENTED_EDGE ( 'NONE', *, *, #21933, .T. ) ;
#20084 = VECTOR ( 'NONE', #4582, 39.37007874015748143 ) ;
#20085 = CARTESIAN_POINT ( 'NONE',  ( 0.3267728913538971991, -0.3414772273308539496, 0.4269974078869066547 ) ) ;
#20086 = EDGE_CURVE ( 'NONE', #9562, #20417, #21931, .T. ) ;
#20087 = CARTESIAN_POINT ( 'NONE',  ( -0.2923287055106771337, 0.3937499999024575148, 0.2123892367102619971 ) ) ;
#20088 = CARTESIAN_POINT ( 'NONE',  ( 0.1167790944451423119, 0.2819444443685777957, -0.2819296736111110979 ) ) ;
#20089 = CARTESIAN_POINT ( 'NONE',  ( 0.2764156081756484196, -5.077672346800151106E-17, 0.3452777777777816803 ) ) ;
#20090 = CARTESIAN_POINT ( 'NONE',  ( 5.178964085587577574E-17, 5.213972222298088433, 0.2819296736111110979 ) ) ;
#20091 = CARTESIAN_POINT ( 'NONE',  ( 0.05308315351926259917, 4.486801226741740756, -0.3074512618920948182 ) ) ;
#20092 = VERTEX_POINT ( 'NONE', #4469 ) ;
#20093 = LINE ( 'NONE', #2814, #7417 ) ;
#20094 = CARTESIAN_POINT ( 'NONE',  ( -0.002508478379659685818, 4.599461472648869176, -0.3119924374546728663 ) ) ;
#20095 = FACE_OUTER_BOUND ( 'NONE', #9224, .T. ) ;
#20096 = CC_DESIGN_APPROVAL ( #21485, ( #8009 ) ) ;
#20097 = CARTESIAN_POINT ( 'NONE',  ( 0.000000000000000000, 5.072999999999999510, 0.000000000000000000 ) ) ;
#20098 = CARTESIAN_POINT ( 'NONE',  ( 0.1292346314604056745, 0.5770833331816004330, -0.3119999999999999996 ) ) ;
#20099 = CARTESIAN_POINT ( 'NONE',  ( 0.2206173157302028787, 4.793833333333332725, 0.2206173157302027954 ) ) ;
#20100 = CARTESIAN_POINT ( 'NONE',  ( -0.1167790944451423119, 3.953555555631421470, -0.2819296736111110979 ) ) ;
#20101 = CARTESIAN_POINT ( 'NONE',  ( 0.2819296736111110979, 3.838972222298087544, -3.452642723725051716E-17 ) ) ;
#20102 = CARTESIAN_POINT ( 'NONE',  ( 0.2944344138913315145, 4.032913573979330479, -0.1032379509715019711 ) ) ;
#20103 = CARTESIAN_POINT ( 'NONE',  ( -0.009375000000000199146, 0.5358532185916217161, 0.3779506566538943790 ) ) ;
#20104 = ORIENTED_EDGE ( 'NONE', *, *, #16183, .T. ) ;
#20105 = AXIS2_PLACEMENT_3D ( 'NONE', #10940, #18368, #23384 ) ;
#20106 = CARTESIAN_POINT ( 'NONE',  ( 0.1294417382415921358, -0.3125000000000002220, 0.1334722222222242682 ) ) ;
#20107 = CARTESIAN_POINT ( 'NONE',  ( 0.1993543840281266633, 4.443138888964754507, -0.1993543840281266910 ) ) ;
#20108 = CARTESIAN_POINT ( 'NONE',  ( 0.3119999999999999996, 3.804249999999999243, -0.1292346314604056745 ) ) ;
#20109 = CARTESIAN_POINT ( 'NONE',  ( 0.1678627478218750191, 0.06466217769286664030, 0.2733718836385306550 ) ) ;
#20110 = CARTESIAN_POINT ( 'NONE',  ( 0.1954553509668047195, 0.1954553509668046085, 0.3452777777777817358 ) ) ;
#20111 = CARTESIAN_POINT ( 'NONE',  ( -1.726321361862525858E-17, 3.797305555631421470, -0.2819296736111110979 ) ) ;
#20112 = CARTESIAN_POINT ( 'NONE',  ( 0.3613381517857143232, 0.4401785713310289450, 0.000000000000000000 ) ) ;
#20113 = CARTESIAN_POINT ( 'NONE',  ( 0.4648120342697257823, 0.2865046371989116714, 0.04342012612512784198 ) ) ;
#20114 = EDGE_CURVE ( 'NONE', #22427, #17016, #22728, .T. ) ;
#20115 = CARTESIAN_POINT ( 'NONE',  ( 0.01848103877824613592, -0.5441716683897390716, 0.04413116910601658227 ) ) ;
#20116 = CARTESIAN_POINT ( 'NONE',  ( -0.2923287055106771337, -0.03125000009754239777, -0.2123892367102620804 ) ) ;
#20117 = CARTESIAN_POINT ( 'NONE',  ( 0.1993543840281266355, 0.3618055554796889006, 0.1993543840281267465 ) ) ;
#20118 = CARTESIAN_POINT ( 'NONE',  ( 0.004465723772902090855, 3.877046577749164502, -0.3119726078432636940 ) ) ;
#20119 = LINE ( 'NONE', #12704, #23617 ) ;
#20120 = CARTESIAN_POINT ( 'NONE',  ( -0.2102330194709680078, 0.3429979575999043684, -0.7199360985034549687 ) ) ;
#20121 = CARTESIAN_POINT ( 'NONE',  ( -3.385114897866767815E-17, -0.2764156081756484196, 0.04666666666666822311 ) ) ;
#20122 = CARTESIAN_POINT ( 'NONE',  ( 0.1954553509668047195, 0.1954553509668046085, -0.09222222222222178911 ) ) ;
#20123 = VERTEX_POINT ( 'NONE', #12053 ) ;
#20124 = CARTESIAN_POINT ( 'NONE',  ( -0.2472135954999579999, 0.08928571428571424606, 0.3402603233408160732 ) ) ;
#20125 = CARTESIAN_POINT ( 'NONE',  ( -0.1292346314604056745, 4.707027777777776478, -0.3119999999999999996 ) ) ;
#20126 = CARTESIAN_POINT ( 'NONE',  ( 0.3119999999999999996, 0.1326388888888885287, -0.1292346314604056468 ) ) ;
#20127 = CARTESIAN_POINT ( 'NONE',  ( 0.1993543840281267465, 3.776472222298087988, 0.1993543840281266633 ) ) ;
#20128 = CARTESIAN_POINT ( 'NONE',  ( -0.2233192592356399997, 0.2008928570453147322, 0.3073725909049499494 ) ) ;
#20129 = EDGE_LOOP ( 'NONE', ( #11857, #11882, #13782, #8601, #17860 ) ) ;
#20130 = CARTESIAN_POINT ( 'NONE',  ( 0.2819296736111110979, 4.502166666742532186, 0.1167790944451422425 ) ) ;
#20131 = CARTESIAN_POINT ( 'NONE',  ( 0.1292346314603994850, 4.977861111111109516, -0.3120000000000061058 ) ) ;
#20132 = ADVANCED_FACE ( 'NONE', ( #8243 ), #12783, .T. ) ;
#20133 = CARTESIAN_POINT ( 'NONE',  ( 0.000000000000000000, 0.04579999999999925103, 0.000000000000000000 ) ) ;
#20134 = ORIENTED_EDGE ( 'NONE', *, *, #13527, .F. ) ;
#20135 = CARTESIAN_POINT ( 'NONE',  ( 0.2984505573353404273, 4.360600408414049056, 0.09256242935286859708 ) ) ;
#20136 = EDGE_CURVE ( 'NONE', #5797, #18537, #4055, .T. ) ;
#20137 = CARTESIAN_POINT ( 'NONE',  ( 0.1167790944451424368, 5.148000000075865223, 0.2819296736111110424 ) ) ;
#20138 = CARTESIAN_POINT ( 'NONE',  ( 0.2318695005579780033, 4.203111999684435496, -0.2087629577079343768 ) ) ;
#20139 = VECTOR ( 'NONE', #13574, 39.37007874015748143 ) ;
#20140 = AXIS2_PLACEMENT_3D ( 'NONE', #4073, #13606, #7618 ) ;
#20141 =( CONVERSION_BASED_UNIT ( 'INCH', #1366 ) LENGTH_UNIT ( ) NAMED_UNIT ( #577 ) );
#20142 = CC_DESIGN_PERSON_AND_ORGANIZATION_ASSIGNMENT ( #5561, #5100, ( #14477 ) ) ;
#20143 = DIRECTION ( 'NONE',  ( 0.000000000000000000, 0.000000000000000000, 1.000000000000000000 ) ) ;
#20144 = CARTESIAN_POINT ( 'NONE',  ( -0.1993543840281266910, 4.845916666742532186, -0.1993543840281266910 ) ) ;
#20145 = CARTESIAN_POINT ( 'NONE',  ( -0.1873832016899178166, 4.065874456094106471, 0.2496566584368918318 ) ) ;
#20146 = CARTESIAN_POINT ( 'NONE',  ( -0.1292346314604058410, 0.4381944442927114824, 0.3119999999999998885 ) ) ;
#20147 = ORIENTED_EDGE ( 'NONE', *, *, #17351, .F. ) ;
#20148 = CARTESIAN_POINT ( 'NONE',  ( 0.1993543840281266910, 0.3340277777019111660, -0.1993543840281266910 ) ) ;
#20149 = CARTESIAN_POINT ( 'NONE',  ( 0.1167790944451423535, 0.2055555554796889006, 0.2819296736111110424 ) ) ;
#20150 = DIRECTION ( 'NONE',  ( 1.000000000000000000, 0.000000000000000000, -6.148297094540788948E-16 ) ) ;
#20151 = CARTESIAN_POINT ( 'NONE',  ( -0.2081355123581232758, 5.196100638220133128, -0.1976311321815438227 ) ) ;
#20152 = CARTESIAN_POINT ( 'NONE',  ( 0.2472135954999579721, -0.01785714285714287697, -0.3402603233408159622 ) ) ;
#20153 = FACE_OUTER_BOUND ( 'NONE', #9434, .T. ) ;
#20154 = CARTESIAN_POINT ( 'NONE',  ( 0.6211549996190571798, 7.606954820578536342E-17, -0.1012499999999999928 ) ) ;
#20155 = CARTESIAN_POINT ( 'NONE',  ( -0.2841659888207613283, 3.887232178795674287, -0.1299132057024031117 ) ) ;
#20156 = CARTESIAN_POINT ( 'NONE',  ( 1.110389585751016872, 2.315961009048385755, -1.013529223733381057 ) ) ;
#20157 = CARTESIAN_POINT ( 'NONE',  ( 0.1993543840281267465, 4.498694444520309865, 0.1993543840281266633 ) ) ;
#20158 = VECTOR ( 'NONE', #4232, 39.37007874015748143 ) ;
#20159 = CARTESIAN_POINT ( 'NONE',  ( 0.4000000000000000222, -0.03750000019508477334, 0.000000000000000000 ) ) ;
#20160 = CARTESIAN_POINT ( 'NONE',  ( 0.3084280012298056262, 4.528428812793057645, 0.05274586746176852803 ) ) ;
#20161 = CARTESIAN_POINT ( 'NONE',  ( -0.1167790944451423535, 5.099388888964754507, 0.2819296736111110424 ) ) ;
#20162 = CARTESIAN_POINT ( 'NONE',  ( 0.4687500000000002776, 0.08745190237456319793, 0.08858760123954047272 ) ) ;
#20163 = EDGE_CURVE ( 'NONE', #11248, #4141, #22360, .T. ) ;
#20164 = CARTESIAN_POINT ( 'NONE',  ( 0.3039537214805487775, 4.921172874434618372, -0.08137803535339727112 ) ) ;
#20165 = LINE ( 'NONE', #16268, #9792 ) ;
#20166 = CARTESIAN_POINT ( 'NONE',  ( -0.1961225106001744101, 0.4280344930761185163, 0.09139053646027218980 ) ) ;
#20167 = EDGE_CURVE ( 'NONE', #9441, #3702, #13113, .T. ) ;
#20168 = CARTESIAN_POINT ( 'NONE',  ( 0.2206173157302027954, 4.259111111262843252, -0.2206173157302028232 ) ) ;
#20169 = CARTESIAN_POINT ( 'NONE',  ( 0.1993543840281267465, 4.554250000075866112, 0.1993543840281266633 ) ) ;
#20170 = CARTESIAN_POINT ( 'NONE',  ( -0.2819296736111110424, 3.856333333409198705, 0.1167790944451424923 ) ) ;
#20171 = ORIENTED_EDGE ( 'NONE', *, *, #9517, .F. ) ;
#20172 = EDGE_CURVE ( 'NONE', #8965, #12281, #7837, .T. ) ;
#20173 = ORIENTED_EDGE ( 'NONE', *, *, #19008, .T. ) ;
#20174 = AXIS2_PLACEMENT_3D ( 'NONE', #18183, #1477, #4650 ) ;
#20175 = EDGE_LOOP ( 'NONE', ( #889, #9721, #2267, #4812 ) ) ;
#20176 = APPLICATION_PROTOCOL_DEFINITION ( 'international standard', 'config_control_design', 1994, #2656 ) ;
#20177 = CARTESIAN_POINT ( 'NONE',  ( -0.2491417453393007519, 4.952411878662227096, 0.1921816384585380566 ) ) ;
#20178 = CARTESIAN_POINT ( 'NONE',  ( -0.5116234456863258950, 2.853030769935284372, -2.756251211572797288 ) ) ;
#20179 = ORIENTED_EDGE ( 'NONE', *, *, #11413, .T. ) ;
#20180 = CARTESIAN_POINT ( 'NONE',  ( 0.3119999999999999996, 0.1777777776260448250, 0.000000000000000000 ) ) ;
#20181 = DIRECTION ( 'NONE',  ( -0.5000000000000037748, 0.000000000000000000, -0.8660254037844362651 ) ) ;
#20182 = CARTESIAN_POINT ( 'NONE',  ( -0.2147042302794207880, 3.717251267640226065, -0.2264494125071482844 ) ) ;
#20183 = CARTESIAN_POINT ( 'NONE',  ( -3.827021247335479543E-17, -0.3125000000000000000, -0.09222222222222198340 ) ) ;
#20184 = CARTESIAN_POINT ( 'NONE',  ( 1.573500000000000343, 0.000000000000000000, -1.412500000000000089 ) ) ;
#20185 = VERTEX_POINT ( 'NONE', #9673 ) ;
#20186 = CARTESIAN_POINT ( 'NONE',  ( 0.2923287055106771337, 0.2330357141881718719, -0.2123892367102620249 ) ) ;
#20187 = ORIENTED_EDGE ( 'NONE', *, *, #4151, .T. ) ;
#20188 = CARTESIAN_POINT ( 'NONE',  ( 0.2385176312641979768, 5.092063675167946002, -0.2011546486555612634 ) ) ;
#20189 = CARTESIAN_POINT ( 'NONE',  ( -0.1144950937579609779, 0.2764156081756484196, 0.3001388888888924522 ) ) ;
#20190 = CARTESIAN_POINT ( 'NONE',  ( -0.1993543840281266910, 4.290361111186976828, -0.1993543840281266910 ) ) ;
#20191 = CARTESIAN_POINT ( 'NONE',  ( 0.2819296736111110979, 5.050777777853643791, -0.1167790944451423396 ) ) ;
#20192 = DIRECTION ( 'NONE',  ( 0.000000000000000000, 0.000000000000000000, 1.000000000000000000 ) ) ;
#20193 = CARTESIAN_POINT ( 'NONE',  ( -0.3119999999999999996, 0.3722222220704893281, -3.820898013339742174E-17 ) ) ;
#20194 = EDGE_CURVE ( 'NONE', #16705, #8965, #7599, .T. ) ;
#20195 = CARTESIAN_POINT ( 'NONE',  ( 0.2206173157302027954, 3.974388888888888083, -0.2206173157302028232 ) ) ;
#20196 = EDGE_CURVE ( 'NONE', #22114, #5871, #20529, .T. ) ;
#20197 = CARTESIAN_POINT ( 'NONE',  ( -0.2206173157302028232, 4.939666666818398610, -0.2206173157302028232 ) ) ;
#20198 = CARTESIAN_POINT ( 'NONE',  ( 0.1993543840281266633, 5.068138888964754507, -0.1993543840281266910 ) ) ;
#20199 =( BOUNDED_SURFACE ( )  B_SPLINE_SURFACE ( 3, 2, ( 
 ( #11718, #488, #11844 ),
 ( #15250, #13433, #2566 ),
 ( #10013, #15612, #6334 ),
 ( #21216, #11971, #2328 ),
 ( #13998, #21428, #4716 ),
 ( #11946, #19361, #8344 ),
 ( #6890, #12640, #14634 ),
 ( #22512, #11429, #5587 ),
 ( #22541, #6070, #21422 ),
 ( #4710, #12178, #8486 ) ),
 .UNSPECIFIED., .F., .F., .F. ) 
 B_SPLINE_SURFACE_WITH_KNOTS ( ( 4, 2, 2, 2, 4 ),
 ( 3, 3 ),
 ( 0.04463809143445897354, 0.04796255359614956526, 0.05128701575784016392, 0.05461147791953076258, 0.05793594008122135430 ),
 ( 0.000000000000000000, 1.000000000000000000 ),
 .UNSPECIFIED. ) 
 GEOMETRIC_REPRESENTATION_ITEM ( )  RATIONAL_B_SPLINE_SURFACE ( (
 ( 1.000000000000000000, 0.8285407536241354842, 1.000000000000000000),
 ( 1.000000000000000000, 0.8326168960425578414, 1.000000000000000000),
 ( 1.000000000000000000, 0.8363786027327638761, 1.000000000000000000),
 ( 1.000000000000000000, 0.8417912930203584887, 1.000000000000000000),
 ( 1.000000000000000000, 0.8433923807919373461, 1.000000000000000000),
 ( 1.000000000000000000, 0.8433905099814716921, 1.000000000000000000),
 ( 1.000000000000000000, 0.8417888685871616206, 1.000000000000000000),
 ( 1.000000000000000000, 0.8363766775000033293, 1.000000000000000000),
 ( 1.000000000000000000, 0.8326159398062553674, 1.000000000000000000),
 ( 1.000000000000000000, 0.8285407536241359283, 1.000000000000000000) ) ) 
 REPRESENTATION_ITEM ( '' )  SURFACE ( )  );
#20200 = FACE_OUTER_BOUND ( 'NONE', #6613, .T. ) ;
#20201 = DIRECTION ( 'NONE',  ( -1.000000000000000000, 0.000000000000000000, 0.000000000000000000 ) ) ;
#20202 = EDGE_CURVE ( 'NONE', #20558, #20678, #20428, .T. ) ;
#20203 = CARTESIAN_POINT ( 'NONE',  ( -0.1504393870195933902, 0.05786178725312922377, 0.2687619224414409813 ) ) ;
#20204 = ORIENTED_EDGE ( 'NONE', *, *, #12033, .F. ) ;
#20205 = CARTESIAN_POINT ( 'NONE',  ( -0.2230971623002953874, 0.2230971623002954152, 0.2810416666666702978 ) ) ;
#20206 = CARTESIAN_POINT ( 'NONE',  ( -0.2819296736111110424, 5.023000000075864335, 0.1167790944451424923 ) ) ;
#20207 = AXIS2_PLACEMENT_3D ( 'NONE', #4429, #2614, #21264 ) ;
#20208 = CARTESIAN_POINT ( 'NONE',  ( 2.346281061938968016, 2.740000000000000213, -2.515999999999999570 ) ) ;
#20209 = EDGE_CURVE ( 'NONE', #11982, #11042, #5881, .T. ) ;
#20210 = CARTESIAN_POINT ( 'NONE',  ( 0.3613381517857143232, 0.3544642856167432576, -0.1174058825155740587 ) ) ;
#20211 = CARTESIAN_POINT ( 'NONE',  ( 0.2819296736111110979, 0.2159722221463555858, 0.000000000000000000 ) ) ;
#20212 = CARTESIAN_POINT ( 'NONE',  ( -0.1954553509668046640, 0.1954553509668046918, 0.1994444444444471720 ) ) ;
#20213 = DIRECTION ( 'NONE',  ( -0.000000000000000000, 1.000000000000000000, -0.000000000000000000 ) ) ;
#20214 = CARTESIAN_POINT ( 'NONE',  ( 3.882666666666670707, 0.9466666666666798680, -0.9716666666666702312 ) ) ;
#20215 = ORIENTED_EDGE ( 'NONE', *, *, #23553, .F. ) ;
#20216 = CARTESIAN_POINT ( 'NONE',  ( 0.1993543840281266633, 4.887583333409199149, -0.1993543840281266910 ) ) ;
#20217 = CARTESIAN_POINT ( 'NONE',  ( -0.3120384249108475450, 4.169999822687207036, 0.04055185888031334618 ) ) ;
#20218 = CARTESIAN_POINT ( 'NONE',  ( -0.3119999999999998885, 5.054249999999998799, 0.1292346314604058410 ) ) ;
#20219 = DIRECTION ( 'NONE',  ( 0.000000000000000000, 0.000000000000000000, 1.000000000000000000 ) ) ;
#20220 = CARTESIAN_POINT ( 'NONE',  ( 0.2340640474074713873, 0.06249999999999967387, 0.2102997499711236618 ) ) ;
#20221 = CARTESIAN_POINT ( 'NONE',  ( -0.1292346314604056745, 4.651472222222221120, -0.3119999999999999996 ) ) ;
#20222 = CARTESIAN_POINT ( 'NONE',  ( -0.1167790944451423119, 4.064666666742532186, -0.2819296736111110979 ) ) ;
#20223 = CARTESIAN_POINT ( 'NONE',  ( -0.1167790944451423257, 3.745222222298088433, -0.2819296736111110424 ) ) ;
#20224 = CARTESIAN_POINT ( 'NONE',  ( 0.3026829317664078700, 4.027635661132299205, 0.08109514562084400857 ) ) ;
#20225 = CARTESIAN_POINT ( 'NONE',  ( -0.01848103877824621571, 0.5441716683897389606, 0.04413116910601659615 ) ) ;
#20226 = VERTEX_POINT ( 'NONE', #16986 ) ;
#20227 = VECTOR ( 'NONE', #12929, 39.37007874015748143 ) ;
#20228 = PLANE ( 'NONE',  #18286 ) ;
#20229 = VERTEX_POINT ( 'NONE', #13341 ) ;
#20230 = CARTESIAN_POINT ( 'NONE',  ( 5.178964085587577574E-17, 4.200083333409199149, 0.2819296736111110979 ) ) ;
#20231 = CARTESIAN_POINT ( 'NONE',  ( -0.3142628774615948695, 4.113298624980298968, 0.0008691249496092882118 ) ) ;
#20232 = CARTESIAN_POINT ( 'NONE',  ( 0.3950000000000000178, 0.05000000000000028727, -2.540999999999999925 ) ) ;
#20233 = CARTESIAN_POINT ( 'NONE',  ( -0.1954553509668046918, -0.1954553509668046640, 0.2619444444444477549 ) ) ;
#20234 = CARTESIAN_POINT ( 'NONE',  ( -0.2726213901831366915, 3.951241869235229576, 0.1571290601157238898 ) ) ;
#20235 = CARTESIAN_POINT ( 'NONE',  ( 0.2977100099089716734, 3.700000000000000622, 0.09499999999999995948 ) ) ;
#20236 = SHAPE_REPRESENTATION ( 'Aloris-BXA-Center-Shaft', ( #9127 ), #7955 ) ;
#20237 = CARTESIAN_POINT ( 'NONE',  ( -3.385114897866767815E-17, -0.2764156081756484196, 0.3869444444444486431 ) ) ;
#20238 = CARTESIAN_POINT ( 'NONE',  ( -6.979263641208234666E-17, 0.3508928570453145879, 0.3799334167787516425 ) ) ;
#20239 = AXIS2_PLACEMENT_3D ( 'NONE', #17315, #8040, #16951 ) ;
#20240 = CARTESIAN_POINT ( 'NONE',  ( 0.2819296736111110424, 0.1986111110352444253, 0.1167790944451424923 ) ) ;
#20241 = CARTESIAN_POINT ( 'NONE',  ( -0.3149999999999997802, 0.06786299768266475241, 0.000000000000000000 ) ) ;
#20242 = CARTESIAN_POINT ( 'NONE',  ( 0.2206173157302027676, 0.5666666666666663188, 0.2206173157302028787 ) ) ;
#20243 = CARTESIAN_POINT ( 'NONE',  ( 2.581625566823704254, 0.04999999999999919092, -2.591000000000000636 ) ) ;
#20244 = CARTESIAN_POINT ( 'NONE',  ( 0.000000000000000000, 0.2764156081756484196, -0.08527777777777729995 ) ) ;
#20245 = ORIENTED_EDGE ( 'NONE', *, *, #22626, .T. ) ;
#20246 = EDGE_LOOP ( 'NONE', ( #8777, #2773, #20104, #3396 ) ) ;
#20247 = CARTESIAN_POINT ( 'NONE',  ( -0.1555525600596525115, 5.096577603750602314, -0.2701852920847304662 ) ) ;
#20248 = CARTESIAN_POINT ( 'NONE',  ( 0.4587679940481828589, -0.1778967816146775627, 0.4165814724634111510 ) ) ;
#20249 = CARTESIAN_POINT ( 'NONE',  ( 0.1292346314604056745, 0.02847222222222188515, -0.3119999999999999996 ) ) ;
#20250 = CARTESIAN_POINT ( 'NONE',  ( -0.2819296736111110979, 3.755638888964754951, 0.000000000000000000 ) ) ;
#20251 = CARTESIAN_POINT ( 'NONE',  ( 0.2923287055106771337, 0.2330357141881718719, -0.2123892367102620249 ) ) ;
#20252 = ORIENTED_EDGE ( 'NONE', *, *, #6277, .T. ) ;
#20253 = CARTESIAN_POINT ( 'NONE',  ( 5.178964085587577574E-17, 4.436194444520310753, 0.2819296736111110979 ) ) ;
#20254 = PRODUCT_DEFINITION_SHAPE ( 'NONE', 'NONE',  #24132 ) ;
#20255 = DIRECTION ( 'NONE',  ( 0.8459207832372980240, 0.4883925919151546613, -0.2142211582677908954 ) ) ;
#20256 = CARTESIAN_POINT ( 'NONE',  ( 5.731347020009612645E-17, 4.620222222222221120, 0.3119999999999999996 ) ) ;
#20257 = ORIENTED_EDGE ( 'NONE', *, *, #2467, .F. ) ;
#20258 = CARTESIAN_POINT ( 'NONE',  ( 0.2927819169943106647, 4.360098288153534618, 0.1093008224459383754 ) ) ;
#20259 = CARTESIAN_POINT ( 'NONE',  ( 0.2819296736111110979, 4.932722222298088433, 0.1167790944451422425 ) ) ;
#20260 = EDGE_CURVE ( 'NONE', #20423, #7667, #21017, .T. ) ;
#20261 = AXIS2_PLACEMENT_3D ( 'NONE', #4065, #18591, #16763 ) ;
#20262 = CARTESIAN_POINT ( 'NONE',  ( 0.003964402099250808643, 4.210387593481760504, -0.3119783974053816911 ) ) ;
#20263 = VECTOR ( 'NONE', #20871, 39.37007874015748854 ) ;
#20264 = CARTESIAN_POINT ( 'NONE',  ( -0.2206173157302028787, 0.2194444444444441089, 0.2206173157302027954 ) ) ;
#20265 = CARTESIAN_POINT ( 'NONE',  ( -0.1993543840281266910, 4.568138888964754507, -0.1993543840281266910 ) ) ;
#20266 = DIRECTION ( 'NONE',  ( -0.000000000000000000, -1.000000000000000000, -0.000000000000000000 ) ) ;
#20267 = CARTESIAN_POINT ( 'NONE',  ( 0.4450000000000002842, 0.000000000000000000, -2.540999999999999925 ) ) ;
#20268 = CARTESIAN_POINT ( 'NONE',  ( -0.1167790944451424368, 0.4763888888130221599, 0.2819296736111110424 ) ) ;
#20269 = ORIENTED_EDGE ( 'NONE', *, *, #9690, .T. ) ;
#20270 = CARTESIAN_POINT ( 'NONE',  ( -0.2819296736111110979, 0.3027777777019111660, 0.1167790944451422425 ) ) ;
#20271 = CARTESIAN_POINT ( 'NONE',  ( -1.910449006669871087E-17, 4.203555555555555046, -0.3119999999999999996 ) ) ;
#20272 = CARTESIAN_POINT ( 'NONE',  ( -0.3516234456863465696, 3.856336430858469999, 2.641746252650784665 ) ) ;
#20273 = CARTESIAN_POINT ( 'NONE',  ( 0.2472135954999579721, 0.05357142857142854764, -0.3402603233408159622 ) ) ;
#20274 = CARTESIAN_POINT ( 'NONE',  ( 0.000000000000000000, 0.3155070326520292845, -0.1182638888888888767 ) ) ;
#20275 = CARTESIAN_POINT ( 'NONE',  ( -0.5116234456863258950, 4.559812086079793048, -3.041000364337123507 ) ) ;
#20276 = AXIS2_PLACEMENT_3D ( 'NONE', #16316, #22159, #1796 ) ;
#20277 = CARTESIAN_POINT ( 'NONE',  ( -0.2491303024454969428, 3.885307312177345818, -0.1878477653712340434 ) ) ;
#20278 = CARTESIAN_POINT ( 'NONE',  ( 0.2819296736111110424, -0.01666666674253329886, -0.1167790944451423119 ) ) ;
#20279 = AXIS2_PLACEMENT_3D ( 'NONE', #19666, #19309, #13829 ) ;
#20280 = CARTESIAN_POINT ( 'NONE',  ( 0.2819296736111110979, 4.561194444520310753, -3.452642723725051716E-17 ) ) ;
#20281 = CARTESIAN_POINT ( 'NONE',  ( 0.2472135954999579166, 0.1660714283763436994, 0.3402603233408160732 ) ) ;
#20282 = CARTESIAN_POINT ( 'NONE',  ( 0.2494586801225501804, 4.524212161881605354, 0.1883225769997851351 ) ) ;
#20283 = CARTESIAN_POINT ( 'NONE',  ( 0.2819296736111110979, 5.168833333409199149, 0.1167790944451422425 ) ) ;
#20284 = PRODUCT_RELATED_PRODUCT_CATEGORY ( 'detail', '', ( #14409 ) ) ;
#20285 = CARTESIAN_POINT ( 'NONE',  ( -0.2819296736111110979, 4.460500000075867000, -0.1167790944451422980 ) ) ;
#20286 = FACE_OUTER_BOUND ( 'NONE', #11915, .T. ) ;
#20287 = CARTESIAN_POINT ( 'NONE',  ( 1.910449006669871087E-17, 0.4694444442927115380, -0.3119999999999999996 ) ) ;
#20288 = CARTESIAN_POINT ( 'NONE',  ( -0.4206390790005693492, 0.2984097918724511467, 0.05816431335574642758 ) ) ;
#20289 = CARTESIAN_POINT ( 'NONE',  ( -0.3119999999999998885, 4.338972222373953969, 0.1292346314604058410 ) ) ;
#20290 = CARTESIAN_POINT ( 'NONE',  ( -0.2819296736111110979, 4.474388888964753619, -0.1167790944451422980 ) ) ;
#20291 = CARTESIAN_POINT ( 'NONE',  ( 0.1167790944451422702, 3.835500000075866556, -0.2819296736111110424 ) ) ;
#20292 = ORIENTED_EDGE ( 'NONE', *, *, #19771, .F. ) ;
#20293 = VECTOR ( 'NONE', #19801, 39.37007874015748143 ) ;
#20294 = ORIENTED_EDGE ( 'NONE', *, *, #13082, .F. ) ;
#20295 = PERSON_AND_ORGANIZATION_ROLE ( 'classification_officer' ) ;
#20296 = CARTESIAN_POINT ( 'NONE',  ( 0.4675595609217378934, -0.2849403337939098169, 0.04271891838948285725 ) ) ;
#20297 = CARTESIAN_POINT ( 'NONE',  ( 0.3119999999999999996, 4.248694444444443441, -0.1292346314604056745 ) ) ;
#20298 = LINE ( 'NONE', #22354, #17072 ) ;
#20299 = VERTEX_POINT ( 'NONE', #15164 ) ;
#20300 = CARTESIAN_POINT ( 'NONE',  ( 0.3119999999999999996, 0.2888888887371559577, 0.000000000000000000 ) ) ;
#20301 = CARTESIAN_POINT ( 'NONE',  ( 0.2209708691207961095, -0.2209708691207961651, 0.1994444444444474218 ) ) ;
#20302 = CARTESIAN_POINT ( 'NONE',  ( -0.1658153428128203155, 3.715415045890231749, -0.2660418640364478615 ) ) ;
#20303 = FACE_OUTER_BOUND ( 'NONE', #4302, .T. ) ;
#20304 = CARTESIAN_POINT ( 'NONE',  ( -0.3120000000000000551, 0.4937499999999996336, 0.1292346314604056190 ) ) ;
#20305 = VERTEX_POINT ( 'NONE', #17234 ) ;
#20306 = EDGE_LOOP ( 'NONE', ( #22170, #11222, #7250, #21260, #15885, #6758, #15536, #22633, #19543, #1010, #20622, #11691, #6745, #23771, #15687, #3679, #2626, #9846, #4931, #23260, #11909, #7970, #2550, #2418 ) ) ;
#20307 = CARTESIAN_POINT ( 'NONE',  ( 0.1116596296178199027, 0.2116071427596004639, 0.3436530038418508792 ) ) ;
#20308 = ORIENTED_EDGE ( 'NONE', *, *, #13527, .T. ) ;
#20309 = DIRECTION ( 'NONE',  ( 0.000000000000000000, 0.000000000000000000, 1.000000000000000000 ) ) ;
#20310 = CARTESIAN_POINT ( 'NONE',  ( -0.2764156081756484196, 0.1144950937579609918, 0.3070833333333369830 ) ) ;
#20311 = EDGE_CURVE ( 'NONE', #15814, #2257, #22748, .T. ) ;
#20312 = CARTESIAN_POINT ( 'NONE',  ( 0.1167790944451424368, 4.259111111186975940, 0.2819296736111110424 ) ) ;
#20313 = CARTESIAN_POINT ( 'NONE',  ( 5.178964085587577574E-17, 5.088972222298087544, 0.2819296736111110979 ) ) ;
#20314 = CARTESIAN_POINT ( 'NONE',  ( 0.2944048850341858259, -0.06890421275382911659, 0.4135261689678141894 ) ) ;
#20315 = CARTESIAN_POINT ( 'NONE',  ( -0.1914634726864894720, 4.216274578790281780, -0.2496961836083926023 ) ) ;
#20316 = CARTESIAN_POINT ( 'NONE',  ( 0.3119999999999999996, 3.856333333333332281, -3.820898013339742174E-17 ) ) ;
#20317 = CARTESIAN_POINT ( 'NONE',  ( 0.2206173157302027954, 4.925777777929509327, -0.2206173157302028232 ) ) ;
#20318 = CARTESIAN_POINT ( 'NONE',  ( 0.2672777582604971558, 4.802940054489442723, 0.1621179023351098369 ) ) ;
#20319 = CYLINDRICAL_SURFACE ( 'NONE', #17524, 0.4000000000000000222 ) ;
#20320 = FACE_OUTER_BOUND ( 'NONE', #2654, .T. ) ;
#20321 = DIRECTION ( 'NONE',  ( -0.000000000000000000, -0.000000000000000000, -1.000000000000000000 ) ) ;
#20322 = CARTESIAN_POINT ( 'NONE',  ( 0.2230971623002953874, -0.2230971623002954429, 0.2532638888888922857 ) ) ;
#20323 = CARTESIAN_POINT ( 'NONE',  ( -0.1993543840281266910, 5.179250000075866112, -0.1993543840281266910 ) ) ;
#20324 = EDGE_CURVE ( 'NONE', #428, #4141, #20882, .T. ) ;
#20325 = CARTESIAN_POINT ( 'NONE',  ( 0.3309966345752219374, -0.3501648812924127996, 0.4216785431538761508 ) ) ;
#20326 = CARTESIAN_POINT ( 'NONE',  ( -0.01848103877824600061, -0.5441716683897390716, 0.04413116910601655452 ) ) ;
#20327 = ORIENTED_EDGE ( 'NONE', *, *, #15134, .F. ) ;
#20328 = CARTESIAN_POINT ( 'NONE',  ( -0.1993543840281267465, 0.3062499999241333759, 0.1993543840281266633 ) ) ;
#20329 = CARTESIAN_POINT ( 'NONE',  ( -0.1954553509668046640, 0.1954553509668046918, 0.2550000000000031686 ) ) ;
#20330 = CARTESIAN_POINT ( 'NONE',  ( 0.1993543840281266633, 5.012583333409199149, -0.1993543840281266910 ) ) ;
#20331 = CARTESIAN_POINT ( 'NONE',  ( 0.3131742759023632416, 4.473813942010830047, 0.02214152731887029241 ) ) ;
#20332 = EDGE_CURVE ( 'NONE', #16785, #23140, #7921, .T. ) ;
#20333 = CARTESIAN_POINT ( 'NONE',  ( 5.178964085587577574E-17, 4.922305555631420582, 0.2819296736111110979 ) ) ;
#20334 = CARTESIAN_POINT ( 'NONE',  ( -0.4584512563509609562, 0.2213892873660434080, 0.4064660812447825067 ) ) ;
#20335 =( BOUNDED_CURVE ( )  B_SPLINE_CURVE ( 2, ( #13921, #21467, #19515, #6349, #15625, #17689, #2808, #6588, #14037 ),
 .UNSPECIFIED., .F., .F. ) 
 B_SPLINE_CURVE_WITH_KNOTS ( ( 3, 2, 2, 2, 3 ),
 ( 0.6875000000000000000, 0.6979166666666666297, 0.7083333333333333703, 0.7187500000000000000, 0.7291666666666666297 ),
 .UNSPECIFIED. ) 
 CURVE ( )  GEOMETRIC_REPRESENTATION_ITEM ( )  RATIONAL_B_SPLINE_CURVE ( ( 1.000000000000000000, 0.9238795325112867385, 1.000000000000000000, 0.9238795325112867385, 1.000000000000000000, 0.9238795325112867385, 1.000000000000000000, 0.9238795325112867385, 1.000000000000000000 ) ) 
 REPRESENTATION_ITEM ( '' )  );
#20336 = CARTESIAN_POINT ( 'NONE',  ( -0.1292346314604124191, 5.040361111111109516, -0.3119999999999932272 ) ) ;
#20337 = LINE ( 'NONE', #14865, #23448 ) ;
#20338 = CARTESIAN_POINT ( 'NONE',  ( 4.898587196589413075E-17, 2.735000000000000320, 0.4000000000000000222 ) ) ;
#20339 = CARTESIAN_POINT ( 'NONE',  ( 0.3119999999999999996, 4.415361111111110404, -0.1292346314604056745 ) ) ;
#20340 = CARTESIAN_POINT ( 'NONE',  ( 0.1167790944451424506, 4.036888888964753619, 0.2819296736111110424 ) ) ;
#20341 = CARTESIAN_POINT ( 'NONE',  ( 0.3394572874457115752, 3.700000000000000622, 0.09499999999999993172 ) ) ;
#20342 = CARTESIAN_POINT ( 'NONE',  ( 0.1862751262687404319, 4.021747071989843825, 0.2502911891028875568 ) ) ;
#20343 = CARTESIAN_POINT ( 'NONE',  ( -0.006583558500310001532, 0.5374648580928949038, 0.05971062996525931116 ) ) ;
#20344 = ORIENTED_EDGE ( 'NONE', *, *, #11935, .F. ) ;
#20345 = CARTESIAN_POINT ( 'NONE',  ( 0.2206173157302028787, 3.904944444444443885, 0.2206173157302027954 ) ) ;
#20346 = ORIENTED_EDGE ( 'NONE', *, *, #4838, .F. ) ;
#20347 = CARTESIAN_POINT ( 'NONE',  ( -0.1709082777654523100, 4.122007486075570881, 0.2610300066267514096 ) ) ;
#20348 = AXIS2_PLACEMENT_3D ( 'NONE', #10360, #10236, #6806 ) ;
#20349 = DIRECTION ( 'NONE',  ( -0.000000000000000000, -1.000000000000000000, -0.000000000000000000 ) ) ;
#20350 = CARTESIAN_POINT ( 'NONE',  ( 0.2764156081756483641, -0.1144950937579611167, 0.2237500000000029743 ) ) ;
#20351 = EDGE_CURVE ( 'NONE', #23278, #5903, #13817, .T. ) ;
#20352 = EDGE_CURVE ( 'NONE', #22501, #15771, #8221, .T. ) ;
#20353 = LINE ( 'NONE', #14510, #208 ) ;
#20354 = DIRECTION ( 'NONE',  ( 0.000000000000000000, 0.000000000000000000, 1.000000000000000000 ) ) ;
#20355 = CARTESIAN_POINT ( 'NONE',  ( 0.01833836887202428684, -0.2764156081756484751, 0.3875005808676508789 ) ) ;
#20356 = CARTESIAN_POINT ( 'NONE',  ( 0.1116596296178199027, 0.2830357141881718053, 0.3436530038418508792 ) ) ;
#20357 = CARTESIAN_POINT ( 'NONE',  ( 0.1167790944451423535, 0.1916666665908000333, 0.2819296736111110424 ) ) ;
#20358 = CARTESIAN_POINT ( 'NONE',  ( -5.731347020009612645E-17, 0.2819444444444441089, 0.3119999999999999996 ) ) ;
#20359 = CARTESIAN_POINT ( 'NONE',  ( 0.000000000000000000, 0.000000000000000000, 0.000000000000000000 ) ) ;
#20360 = CARTESIAN_POINT ( 'NONE',  ( -0.1144950937579609779, 0.2764156081756484196, -0.02624999999999906228 ) ) ;
#20361 = EDGE_CURVE ( 'NONE', #12518, #6853, #15643, .T. ) ;
#20362 = ORIENTED_EDGE ( 'NONE', *, *, #15967, .T. ) ;
#20363 = ORIENTED_EDGE ( 'NONE', *, *, #19717, .F. ) ;
#20364 = CARTESIAN_POINT ( 'NONE',  ( -0.05073967362410713305, 5.093467254518128762, -0.3073318483525642741 ) ) ;
#20365 = CARTESIAN_POINT ( 'NONE',  ( 0.4687500000000002776, -0.2598076211353317344, 0.3779506566538943235 ) ) ;
#20366 = CARTESIAN_POINT ( 'NONE',  ( 0.1167790944451423535, 0.5805555554796888451, 0.2819296736111110424 ) ) ;
#20367 = CARTESIAN_POINT ( 'NONE',  ( 0.2819296736111110979, 3.946611111186976384, 0.1167790944451422425 ) ) ;
#20368 = CARTESIAN_POINT ( 'NONE',  ( 0.3613381517857143232, 0.2223214284738861402, 0.1174058825155742114 ) ) ;
#20369 = VERTEX_POINT ( 'NONE', #6489 ) ;
#20370 = VECTOR ( 'NONE', #12354, 39.37007874015748143 ) ;
#20371 = CARTESIAN_POINT ( 'NONE',  ( 0.1993543840281267465, 4.332027777853642903, 0.1993543840281266633 ) ) ;
#20372 = FACE_OUTER_BOUND ( 'NONE', #2992, .T. ) ;
#20373 = LINE ( 'NONE', #1601, #20383 ) ;
#20374 = ORIENTED_EDGE ( 'NONE', *, *, #975, .F. ) ;
#20375 = DIRECTION ( 'NONE',  ( 1.000000000000000000, -0.000000000000000000, 1.224646799147353207E-16 ) ) ;
#20376 = CARTESIAN_POINT ( 'NONE',  ( 0.1993543840281267465, 5.040361111186975940, 0.1993543840281266633 ) ) ;
#20377 = CARTESIAN_POINT ( 'NONE',  ( 9.101228903679513089E-16, 0.3017857140906293756, 0.4000000000000000222 ) ) ;
#20378 =( BOUNDED_CURVE ( )  B_SPLINE_CURVE ( 2, ( #17504, #10446, #13858 ),
 .UNSPECIFIED., .F., .F. ) 
 B_SPLINE_CURVE_WITH_KNOTS ( ( 3, 3 ),
 ( 0.9732142857142858094, 0.9771335280684947389 ),
 .UNSPECIFIED. ) 
 CURVE ( )  GEOMETRIC_REPRESENTATION_ITEM ( )  RATIONAL_B_SPLINE_CURVE ( ( 0.9999999999999981126, 0.9331730585143147572, 0.9836822358325096882 ) ) 
 REPRESENTATION_ITEM ( '' )  );
#20379 = CARTESIAN_POINT ( 'NONE',  ( 1.573500000000000343, 3.744510943477052489, -1.412500000000000089 ) ) ;
#20380 = FACE_OUTER_BOUND ( 'NONE', #16412, .T. ) ;
#20381 = CARTESIAN_POINT ( 'NONE',  ( 0.1167790944451424506, 4.703555555631420582, 0.2819296736111110424 ) ) ;
#20382 = COORDINATED_UNIVERSAL_TIME_OFFSET ( 0, 0, .AHEAD. ) ;
#20383 = VECTOR ( 'NONE', #14287, 39.37007874015748143 ) ;
#20384 = CARTESIAN_POINT ( 'NONE',  ( -0.04741907581679727368, 4.070294630609375908, 0.3093645555771465383 ) ) ;
#20385 = CARTESIAN_POINT ( 'NONE',  ( -0.4805070082343984583, 0.2560807851245828770, 0.04413116910601658921 ) ) ;
#20386 = CARTESIAN_POINT ( 'NONE',  ( -5.178964085587577574E-17, 0.5909722221463555858, 0.2819296736111110979 ) ) ;
#20387 = EDGE_LOOP ( 'NONE', ( #435, #23089, #5443, #285 ) ) ;
#20388 = CARTESIAN_POINT ( 'NONE',  ( -0.1167790944451424368, 0.1986111110352444808, 0.2819296736111110424 ) ) ;
#20389 = ADVANCED_FACE ( 'NONE', ( #1000 ), #21198, .F. ) ;
#20390 = DIRECTION ( 'NONE',  ( 0.000000000000000000, 1.000000000000000000, 0.000000000000000000 ) ) ;
#20391 = DIRECTION ( 'NONE',  ( 1.049727191138617463E-16, -0.5150380749100555988, 0.8571673007021114454 ) ) ;
#20392 = CARTESIAN_POINT ( 'NONE',  ( -7.726019084026502927E-17, 0.2392857142857141295, 0.4205848896953069405 ) ) ;
#20393 = LINE ( 'NONE', #18440, #359 ) ;
#20394 = EDGE_CURVE ( 'NONE', #22303, #22427, #6606, .T. ) ;
#20395 = CARTESIAN_POINT ( 'NONE',  ( -0.4620259694561525965, -0.2880908832651560281, 0.04413116910601649207 ) ) ;
#20396 = CARTESIAN_POINT ( 'NONE',  ( -0.2558214270178758021, 3.885631657198463706, -0.1786047227777496083 ) ) ;
#20397 = CARTESIAN_POINT ( 'NONE',  ( -5.178964085587577574E-17, 0.1881944443685778512, 0.2819296736111110979 ) ) ;
#20398 = CARTESIAN_POINT ( 'NONE',  ( -0.1167790944451424368, 0.01805555547968892838, 0.2819296736111110424 ) ) ;
#20399 = CARTESIAN_POINT ( 'NONE',  ( 0.1167790944451422702, 4.516055555631421470, -0.2819296736111110424 ) ) ;
#20400 = CARTESIAN_POINT ( 'NONE',  ( 0.3236067977499790249, 0.1124999998049151934, -0.2351141009169892826 ) ) ;
#20401 = CARTESIAN_POINT ( 'NONE',  ( 0.1993543840281267465, 5.054250000075865223, 0.1993543840281266633 ) ) ;
#20402 = CARTESIAN_POINT ( 'NONE',  ( -0.1993543840281266910, 4.512583333409199149, -0.1993543840281266910 ) ) ;
#20403 = CARTESIAN_POINT ( 'NONE',  ( 0.1521196438571344733, 3.742789775738293301, 0.2735830517299060460 ) ) ;
#20404 = CARTESIAN_POINT ( 'NONE',  ( 0.3125000000000000000, -5.740531871003217465E-17, 0.1994444444444470055 ) ) ;
#20405 = CARTESIAN_POINT ( 'NONE',  ( 0.3143848286800483005, 3.918459697589230739, 0.01319625459807933707 ) ) ;
#20406 = CARTESIAN_POINT ( 'NONE',  ( -0.1292346314604057023, 4.068138889040620931, 0.3119999999999998885 ) ) ;
#20407 = VECTOR ( 'NONE', #15863, 39.37007874015748143 ) ;
#20408 = CARTESIAN_POINT ( 'NONE',  ( -0.1993543840281266355, 4.429250000075866112, 0.1993543840281267465 ) ) ;
#20409 = CARTESIAN_POINT ( 'NONE',  ( -0.4593750000000004219, 0.2760455974562897596, 0.3779506566538943790 ) ) ;
#20410 = VERTEX_POINT ( 'NONE', #12002 ) ;
#20411 = VERTEX_POINT ( 'NONE', #6122 ) ;
#20412 = PERSON_AND_ORGANIZATION ( #15518, #2538 ) ;
#20413 = CARTESIAN_POINT ( 'NONE',  ( -0.04527543151830683288, 4.848148877423151148, 0.3096339228700176749 ) ) ;
#20414 = DIRECTION ( 'NONE',  ( 0.000000000000000000, 0.000000000000000000, 1.000000000000000000 ) ) ;
#20415 = ORIENTED_EDGE ( 'NONE', *, *, #18097, .T. ) ;
#20416 = CARTESIAN_POINT ( 'NONE',  ( 0.2206173157302027676, 0.5041666665149336923, 0.2206173157302028787 ) ) ;
#20417 = VERTEX_POINT ( 'NONE', #14054 ) ;
#20418 = DIRECTION ( 'NONE',  ( -0.000000000000000000, -0.9961946980917454342, 0.08715574274765830465 ) ) ;
#20419 = CARTESIAN_POINT ( 'NONE',  ( -0.1342463367781699390, 3.734338305776751188, 0.2818767121370694961 ) ) ;
#20420 = VECTOR ( 'NONE', #20497, 39.37007874015748143 ) ;
#20421 = CARTESIAN_POINT ( 'NONE',  ( 1.585131139260598010, 2.978485840173427324, -2.498788568296995916 ) ) ;
#20422 = DIRECTION ( 'NONE',  ( 0.000000000000000000, 0.7071067811865474617, 0.7071067811865474617 ) ) ;
#20423 = VERTEX_POINT ( 'NONE', #11752 ) ;
#20424 = CARTESIAN_POINT ( 'NONE',  ( -0.3613381517857143232, 0.04374999990245761333, -0.1174058825155741143 ) ) ;
#20425 = VERTEX_POINT ( 'NONE', #19175 ) ;
#20426 = CARTESIAN_POINT ( 'NONE',  ( 0.3116113683979374605, 5.085271449707127189, 0.01361995752066778517 ) ) ;
#20427 = CARTESIAN_POINT ( 'NONE',  ( -0.1144950937579609779, 0.2764156081756484196, 0.3556944444444484765 ) ) ;
#20428 =( BOUNDED_CURVE ( )  B_SPLINE_CURVE ( 2, ( #2111, #11509, #22598, #19057, #18944, #7950, #9801, #5770, #13231, #20643, #18579, #1869, #15282 ),
 .UNSPECIFIED., .F., .T. ) 
 B_SPLINE_CURVE_WITH_KNOTS ( ( 3, 2, 2, 2, 2, 2, 3 ),
 ( 0.6071428571428572063, 0.6142857142857143238, 0.6285714285714285587, 0.6428571428571429047, 0.6571428571428571397, 0.6714285714285713746, 0.6785714285714286031 ),
 .UNSPECIFIED. ) 
 CURVE ( )  GEOMETRIC_REPRESENTATION_ITEM ( )  RATIONAL_B_SPLINE_CURVE ( ( 0.9755282581475768211, 0.9755282581475769321, 1.000000000000000000, 0.9510565162951535312, 1.000000000000000000, 0.9510565162951535312, 1.000000000000000000, 0.9510565162951535312, 1.000000000000000000, 0.9510565162951535312, 1.000000000000000000, 0.9755282581475765991, 0.9755282581475768211 ) ) 
 REPRESENTATION_ITEM ( '' )  );
#20429 = CARTESIAN_POINT ( 'NONE',  ( -0.2819296736111110424, 4.245222222298087544, 0.1167790944451424923 ) ) ;
#20430 = CARTESIAN_POINT ( 'NONE',  ( -1.726321361862525858E-17, 5.172305555631420582, -0.2819296736111110979 ) ) ;
#20431 = CARTESIAN_POINT ( 'NONE',  ( -0.04282247326132401083, -0.5165423109005167213, 0.4011144384304581867 ) ) ;
#20432 = CARTESIAN_POINT ( 'NONE',  ( -0.3125000000000000000, 0.000000000000000000, 1.326383476483184332 ) ) ;
#20433 = CARTESIAN_POINT ( 'NONE',  ( 0.1123264932791805809, 3.756093169699425083, -0.3119999999999999996 ) ) ;
#20434 = CARTESIAN_POINT ( 'NONE',  ( -0.3119999999999999996, 4.665361111262842364, -0.1292346314604056468 ) ) ;
#20435 = CARTESIAN_POINT ( 'NONE',  ( 0.2819296736111110979, 5.116750000075866112, -3.452642723725051716E-17 ) ) ;
#20436 = B_SPLINE_CURVE_WITH_KNOTS ( 'NONE', 3,
 ( #4625, #10251, #12090, #19500, #2796, #965, #14025, #6093, #19619, #9767, #489, #11720, #19143, #9890, #17318, #1573, #10849, #22051, #3155, #19985, #8642, #14628, #5217, #6693, #21808, #10725, #17918, #18035, #14380, #23740, #6940, #7065, #5097, #14504, #1331, #1090, #19860, #12811, #12327, #16452, #8757, #18157, #23625, #18278, #19741, #23866, #2916, #9009, #16330, #8522, #14138, #12564, #16213, #1454, #3272, #7186, #8887, #5347 ),
 .UNSPECIFIED., .F., .F.,
 ( 4, 2, 1, 2, 2, 1, 1, 1, 1, 2, 2, 2, 1, 1, 1, 2, 2, 2, 2, 2, 2, 2, 1, 2, 2, 1, 2, 2, 2, 2, 2, 2, 2, 4 ),
 ( 0.4648409156512180451, 0.4660563802132510758, 0.4663602463537592779, 0.4665121794240134068, 0.4665216752409043210, 0.4665311710577951798, 0.4665501626915769529, 0.4665881459591404989, 0.4666641124942675911, 0.4672718447752841620, 0.4697027738993504453, 0.4709182384613835870, 0.4710701715316377158, 0.4711461380667647525, 0.4711841213343282986, 0.4712031129681100716, 0.4712221046018918447, 0.4715259707424001023, 0.4721337030234166732, 0.4733491675854497038, 0.4745646321474827900, 0.4757800967095158762, 0.4758560632446429128, 0.4758940465122064589, 0.4759320297797700050, 0.4760839628500241338, 0.4763878289905323915, 0.4769955612715489068, 0.4794264903956150792, 0.4818574195196811960, 0.4830728840817142822, 0.4836806163627308530, 0.4839844825032391107, 0.4842883486437473683 ),
 .UNSPECIFIED. ) ;
#20437 = ORIENTED_EDGE ( 'NONE', *, *, #19318, .F. ) ;
#20438 = CARTESIAN_POINT ( 'NONE',  ( 0.2923287055106771337, 0.1294642856167433076, 0.2123892367102621359 ) ) ;
#20439 = AXIS2_PLACEMENT_3D ( 'NONE', #11424, #22749, #2397 ) ;
#20440 = CARTESIAN_POINT ( 'NONE',  ( 0.2195746668131363655, 0.03828721274327267360, -0.1863886668264715940 ) ) ;
#20441 = PERSON_AND_ORGANIZATION ( #15518, #2538 ) ;
#20442 = APPROVAL ( #15285, 'UNSPECIFIED' ) ;
#20443 = CARTESIAN_POINT ( 'NONE',  ( -0.1306872919485614903, 0.3155070326520293400, 0.2220138888888920359 ) ) ;
#20444 = CARTESIAN_POINT ( 'NONE',  ( -0.2819296736111110979, 5.186194444520309865, 0.000000000000000000 ) ) ;
#20445 = CC_DESIGN_APPROVAL ( #23394, ( #8363 ) ) ;
#20446 = VERTEX_POINT ( 'NONE', #21369 ) ;
#20447 = CARTESIAN_POINT ( 'NONE',  ( 0.006542161132012845430, -0.5374887588746249945, 0.3892820121258430133 ) ) ;
#20448 = PRODUCT_DEFINITION_SHAPE ( 'NONE', 'NONE',  #24137 ) ;
#20449 = FACE_OUTER_BOUND ( 'NONE', #5439, .T. ) ;
#20450 = CARTESIAN_POINT ( 'NONE',  ( 0.2819296736111110424, 0.2680555554796889561, 0.1167790944451424923 ) ) ;
#20451 = CARTESIAN_POINT ( 'NONE',  ( -3.385114897866767815E-17, -0.2764156081756484196, 0.2758333333333366499 ) ) ;
#20452 = CARTESIAN_POINT ( 'NONE',  ( -0.2819296736111110424, 5.036888888964754507, 0.1167790944451424923 ) ) ;
#20453 = CARTESIAN_POINT ( 'NONE',  ( 0.08714812177476737032, 4.485845587538219270, -0.2997357158451462444 ) ) ;
#20454 = CIRCLE ( 'NONE', #11513, 0.2510000000000000009 ) ;
#20455 = CARTESIAN_POINT ( 'NONE',  ( 0.2819296736111110979, 4.991750000075866112, -3.452642723725051716E-17 ) ) ;
#20456 = CARTESIAN_POINT ( 'NONE',  ( -0.4593750000000003664, 0.04475449550936177329, 0.4343810118395208253 ) ) ;
#20457 = CARTESIAN_POINT ( 'NONE',  ( 1.840071746775174377, 2.291712385858714729, -2.386288568296997425 ) ) ;
#20458 = CARTESIAN_POINT ( 'NONE',  ( 0.1292346314604068680, 4.588972222222221120, -0.3119999999999987228 ) ) ;
#20459 = CARTESIAN_POINT ( 'NONE',  ( 1.850761986253052660, 2.471736157945122692, -1.938010564379532674 ) ) ;
#20460 = CARTESIAN_POINT ( 'NONE',  ( 0.2206173157302028787, 4.571611111111110404, 0.2206173157302027954 ) ) ;
#20461 = CARTESIAN_POINT ( 'NONE',  ( 0.2819296736111110979, 3.936194444520309865, -3.452642723725051716E-17 ) ) ;
#20462 = DIRECTION ( 'NONE',  ( -1.000000000000000000, 0.000000000000000000, 0.000000000000000000 ) ) ;
#20463 = CARTESIAN_POINT ( 'NONE',  ( 0.2348144578000487537, 4.023596968965510889, 0.2061937808865371424 ) ) ;
#20464 = CARTESIAN_POINT ( 'NONE',  ( 0.000000000000000000, 5.384999999999999787, 0.000000000000000000 ) ) ;
#20465 = APPROVAL_PERSON_ORGANIZATION ( #23688, #14947, #8954 ) ;
#20466 = LINE ( 'NONE', #3517, #9330 ) ;
#20467 = VERTEX_POINT ( 'NONE', #22944 ) ;
#20468 = EDGE_CURVE ( 'NONE', #13845, #21793, #19625, .T. ) ;
#20469 = CARTESIAN_POINT ( 'NONE',  ( -0.1756959055429883343, 4.121843226292245532, 0.2578300476179096190 ) ) ;
#20470 = VECTOR ( 'NONE', #20061, 39.37007874015748143 ) ;
#20471 = EDGE_CURVE ( 'NONE', #11997, #14781, #5223, .T. ) ;
#20472 = CARTESIAN_POINT ( 'NONE',  ( 0.2562267853273828555, 4.635683002082432225, 0.1824161936367395542 ) ) ;
#20473 = CARTESIAN_POINT ( 'NONE',  ( -0.1144950937579609918, -0.2764156081756484196, 0.2654166666666700203 ) ) ;
#20474 = DIRECTION ( 'NONE',  ( -0.000000000000000000, -1.000000000000000000, -0.000000000000000000 ) ) ;
#20475 = CARTESIAN_POINT ( 'NONE',  ( 8.984713656453739555E-13, 5.162518060853549251, -0.2988821118451543968 ) ) ;
#20476 = CC_DESIGN_APPROVAL ( #23253, ( #3736 ) ) ;
#20477 = CARTESIAN_POINT ( 'NONE',  ( -0.3613381517857144343, 0.3366071427596004084, 0.1174058825155740171 ) ) ;
#20478 = CARTESIAN_POINT ( 'NONE',  ( 0.2819296736111110424, 0.2055555554796889006, -0.1167790944451423119 ) ) ;
#20479 = CARTESIAN_POINT ( 'NONE',  ( 0.1005328971134487603, 3.874363271045468071, -0.2960644379690948180 ) ) ;
#20480 = DIRECTION ( 'NONE',  ( 0.000000000000000000, 0.000000000000000000, -1.000000000000000000 ) ) ;
#20481 = CARTESIAN_POINT ( 'NONE',  ( 0.3856318672988792162, 0.3186212149721686648, 0.4002893343786020353 ) ) ;
#20482 = CARTESIAN_POINT ( 'NONE',  ( -3.385114897866767815E-17, -0.2764156081756484196, -0.05749999999999930167 ) ) ;
#20483 = CARTESIAN_POINT ( 'NONE',  ( 0.08808798601667688910, 4.111524471938507119, -3.348023836630494632 ) ) ;
#20484 = CARTESIAN_POINT ( 'NONE',  ( 0.4687500000000002776, -0.04376700804269017392, 0.4181543355204243584 ) ) ;
#20485 = CARTESIAN_POINT ( 'NONE',  ( 0.3119999999999999996, 0.07708333333333300397, -0.1292346314604056468 ) ) ;
#20486 = CARTESIAN_POINT ( 'NONE',  ( 0.3119999999999999996, 5.137583333333332725, -0.1292346314604056745 ) ) ;
#20487 = CARTESIAN_POINT ( 'NONE',  ( 0.1116596296178199860, 0.1687499999024575925, -0.3436530038418508792 ) ) ;
#20488 = ORIENTED_EDGE ( 'NONE', *, *, #1089, .F. ) ;
#20489 = CARTESIAN_POINT ( 'NONE',  ( 0.1993543840281266633, 4.123694444520309865, -0.1993543840281266910 ) ) ;
#20490 = CARTESIAN_POINT ( 'NONE',  ( 0.3308333333333332571, 3.738758431839877614E-19, 0.4425000000000000044 ) ) ;
#20491 = CARTESIAN_POINT ( 'NONE',  ( 0.3084175934503982641, -2.427762526784286478E-18, -0.1882653658700420007 ) ) ;
#20492 = ORIENTED_EDGE ( 'NONE', *, *, #2869, .T. ) ;
#20493 = ADVANCED_FACE ( 'NONE', ( #10044 ), #19533, .T. ) ;
#20494 = CARTESIAN_POINT ( 'NONE',  ( 0.2479582629286654072, 4.357447403414685283, 0.1904730091441463047 ) ) ;
#20495 = CARTESIAN_POINT ( 'NONE',  ( -0.2819296736111110424, 4.967444444520310753, 0.1167790944451424923 ) ) ;
#20496 = LOCAL_TIME ( 21, 9, 13.00000000000000000, #11362 ) ;
#20497 = DIRECTION ( 'NONE',  ( 0.000000000000000000, -0.9961946980917454342, -0.08715574274765833240 ) ) ;
#20498 = EDGE_CURVE ( 'NONE', #4780, #22531, #1720, .T. ) ;
#20499 = CARTESIAN_POINT ( 'NONE',  ( 0.007859944718908516703, 3.710288412741159725, -0.3119151351536944006 ) ) ;
#20500 = CARTESIAN_POINT ( 'NONE',  ( -0.2206173157302027954, 0.2055555555555551861, -0.2206173157302028232 ) ) ;
#20501 = AXIS2_PLACEMENT_3D ( 'NONE', #5101, #12815, #3521 ) ;
#20502 = CARTESIAN_POINT ( 'NONE',  ( 0.1993543840281266633, 4.776472222298087544, -0.1993543840281266910 ) ) ;
#20503 = APPROVAL_ROLE ( '' ) ;
#20504 = CARTESIAN_POINT ( 'NONE',  ( -0.1492905759043549330, 4.067176878490561975, 0.2739898953200897158 ) ) ;
#20505 = CARTESIAN_POINT ( 'NONE',  ( -0.3125000000000000000, 1.913510623667739771E-17, -0.05055555555555497210 ) ) ;
#20506 = CARTESIAN_POINT ( 'NONE',  ( 0.1993543840281266355, 0.4312499999241333759, 0.1993543840281267465 ) ) ;
#20507 = VERTEX_POINT ( 'NONE', #21484 ) ;
#20508 = ORIENTED_EDGE ( 'NONE', *, *, #6540, .T. ) ;
#20509 = CARTESIAN_POINT ( 'NONE',  ( 1.726321361862525858E-17, 0.2298611110352444531, -0.2819296736111110979 ) ) ;
#20510 = LINE ( 'NONE', #12, #17019 ) ;
#20511 = CARTESIAN_POINT ( 'NONE',  ( -0.1236067977499789583, 0.3410714283763437438, -0.3804226065180614791 ) ) ;
#20512 = CARTESIAN_POINT ( 'NONE',  ( 0.1236067977499789028, 0.2428571428571427715, 0.3804226065180614791 ) ) ;
#20513 = CARTESIAN_POINT ( 'NONE',  ( -0.3155070326520293400, -0.1306872919485614626, 0.01020833333333438092 ) ) ;
#20514 = CARTESIAN_POINT ( 'NONE',  ( -3.827021247335479543E-17, -0.3125000000000000000, 0.02583333333333490481 ) ) ;
#20515 = DIRECTION ( 'NONE',  ( -0.5000000000000037748, 0.000000000000000000, -0.8660254037844362651 ) ) ;
#20516 = CARTESIAN_POINT ( 'NONE',  ( 0.1167790944451423119, 0.1569444443685777679, -0.2819296736111110979 ) ) ;
#20517 = CARTESIAN_POINT ( 'NONE',  ( 0.2819296736111110424, 0.03888888881302225708, -0.1167790944451423119 ) ) ;
#20518 = CARTESIAN_POINT ( 'NONE',  ( -0.2819296736111110424, 4.196611111186976828, -0.1167790944451423119 ) ) ;
#20519 = CARTESIAN_POINT ( 'NONE',  ( -0.2472135954999579999, 0.08035714266205805367, 0.3402603233408159622 ) ) ;
#20520 = CARTESIAN_POINT ( 'NONE',  ( -0.2819296736111110979, 5.088972222298087544, 0.000000000000000000 ) ) ;
#20521 = CARTESIAN_POINT ( 'NONE',  ( -0.2819296736111110979, 4.408416666742532186, 0.000000000000000000 ) ) ;
#20522 = CARTESIAN_POINT ( 'NONE',  ( 0.000000000000000000, 5.384999999999999787, 0.000000000000000000 ) ) ;
#20523 = VERTEX_POINT ( 'NONE', #8430 ) ;
#20524 = VECTOR ( 'NONE', #7195, 39.37007874015748143 ) ;
#20525 = CARTESIAN_POINT ( 'NONE',  ( -0.2773501192371494728, 0.3936383244007691240, 0.07440066028687920829 ) ) ;
#20526 = CARTESIAN_POINT ( 'NONE',  ( -0.2206173157302027676, 4.120222222373954857, 0.2206173157302028787 ) ) ;
#20527 =( BOUNDED_CURVE ( )  B_SPLINE_CURVE ( 2, ( #14126, #1075, #6559, #8632, #23489, #12552, #18145, #21555, #2782, #21324, #17663, #4846, #5084 ),
 .UNSPECIFIED., .F., .T. ) 
 B_SPLINE_CURVE_WITH_KNOTS ( ( 3, 2, 2, 2, 2, 2, 3 ),
 ( 0.3928571428571429047, 0.4000000000000000222, 0.4142857142857143127, 0.4285714285714285476, 0.4428571428571428381, 0.4571428571428571286, 0.4642857142857143016 ),
 .UNSPECIFIED. ) 
 CURVE ( )  GEOMETRIC_REPRESENTATION_ITEM ( )  RATIONAL_B_SPLINE_CURVE ( ( 0.9755282581475767101, 0.9755282581475768211, 1.000000000000000000, 0.9510565162951535312, 1.000000000000000000, 0.9510565162951535312, 1.000000000000000000, 0.9510565162951535312, 1.000000000000000000, 0.9510565162951535312, 1.000000000000000000, 0.9755282581475765991, 0.9755282581475767101 ) ) 
 REPRESENTATION_ITEM ( '' )  );
#20528 =( BOUNDED_SURFACE ( )  B_SPLINE_SURFACE ( 3, 2, ( 
 ( #1147, #8695, #21751 ),
 ( #14318, #14443, #12504 ),
 ( #16146, #8454, #3098 ),
 ( #4921, #6999, #6875 ),
 ( #17978, #8586, #12385 ),
 ( #12260, #21867, #1390 ) ),
 .UNSPECIFIED., .F., .F., .T. ) 
 B_SPLINE_SURFACE_WITH_KNOTS ( ( 4, 2, 4 ),
 ( 3, 3 ),
 ( 0.001402224832186923413, 0.001901366090229829071, 0.002400507348272734511 ),
 ( 0.000000000000000000, 1.000000000000000000 ),
 .UNSPECIFIED. ) 
 GEOMETRIC_REPRESENTATION_ITEM ( )  RATIONAL_B_SPLINE_SURFACE ( (
 ( 1.000000000000000000, 0.8285407536241354842, 1.000000000000000000),
 ( 1.000000000000000000, 0.8382697314792872945, 1.000000000000000000),
 ( 1.000000000000000000, 0.8433836253083701884, 1.000000000000000000),
 ( 1.000000000000000000, 0.8433992480895078359, 1.000000000000000000),
 ( 1.000000000000000000, 0.8382827608169546307, 1.000000000000000000),
 ( 1.000000000000000000, 0.8285407536241033988, 1.000000000000000000) ) ) 
 REPRESENTATION_ITEM ( '' )  SURFACE ( )  );
#20529 = LINE ( 'NONE', #11630, #3670 ) ;
#20530 = ADVANCED_FACE ( 'NONE', ( #2482 ), #18877, .T. ) ;
#20531 = CARTESIAN_POINT ( 'NONE',  ( -0.2562433651783130317, -0.1785792061923512919, -0.1010489577189804811 ) ) ;
#20532 = ORIENTED_EDGE ( 'NONE', *, *, #2897, .F. ) ;
#20533 = ORIENTED_EDGE ( 'NONE', *, *, #1550, .T. ) ;
#20534 = COORDINATED_UNIVERSAL_TIME_OFFSET ( 0, 0, .AHEAD. ) ;
#20535 = DIRECTION ( 'NONE',  ( -0.000000000000000000, -1.000000000000000000, -0.000000000000000000 ) ) ;
#20536 = CARTESIAN_POINT ( 'NONE',  ( 0.4581189881604794123, -0.2644951211353317455, 0.3941886329748525153 ) ) ;
#20537 = LINE ( 'NONE', #3833, #11634 ) ;
#20538 = VERTEX_POINT ( 'NONE', #12240 ) ;
#20539 = CARTESIAN_POINT ( 'NONE',  ( 0.3119999999999998885, 0.5631944442927114824, 0.1292346314604058410 ) ) ;
#20540 = AXIS2_PLACEMENT_3D ( 'NONE', #21621, #21745, #3093 ) ;
#20541 = VERTEX_POINT ( 'NONE', #19653 ) ;
#20542 = CARTESIAN_POINT ( 'NONE',  ( -3.827021247335479543E-17, -0.3125000000000000000, 0.1925000000000028910 ) ) ;
#20543 = CARTESIAN_POINT ( 'NONE',  ( 9.326145492192990669E-05, 4.766052907303594210, -0.3120000010180138394 ) ) ;
#20544 = CARTESIAN_POINT ( 'NONE',  ( 0.2923287055106771337, 0.05803571418817188299, 0.2123892367102621359 ) ) ;
#20545 = VERTEX_POINT ( 'NONE', #9917 ) ;
#20546 = CARTESIAN_POINT ( 'NONE',  ( -0.3613381517857143232, 0.1866071427596004140, -0.1174058825155741143 ) ) ;
#20547 = CARTESIAN_POINT ( 'NONE',  ( -1.903245722532910002E-17, 5.100068075568266579, -0.3108236144263021861 ) ) ;
#20548 = CARTESIAN_POINT ( 'NONE',  ( -0.1954553509668046640, 0.1954553509668046918, 0.4702777777777827350 ) ) ;
#20549 = CARTESIAN_POINT ( 'NONE',  ( 0.1167790944451424368, 4.203555555631420582, 0.2819296736111110424 ) ) ;
#20550 = CARTESIAN_POINT ( 'NONE',  ( -0.1993543840281266355, 5.026472222298088433, 0.1993543840281267465 ) ) ;
#20551 = CARTESIAN_POINT ( 'NONE',  ( 0.2659300498200044549, -0.1330428112940453822, 0.4085120587161163996 ) ) ;
#20552 = CARTESIAN_POINT ( 'NONE',  ( -0.2775113281607684557, 0.3935459114639778821, 0.07438423612653367878 ) ) ;
#20553 = CARTESIAN_POINT ( 'NONE',  ( 0.2206173157302027954, 3.863277777777777366, -0.2206173157302028232 ) ) ;
#20554 = CARTESIAN_POINT ( 'NONE',  ( -1.910449006669871087E-17, 4.654944444596176290, -0.3119999999999999996 ) ) ;
#20555 = CARTESIAN_POINT ( 'NONE',  ( -0.1993543840281266910, 5.137583333409199149, -0.1993543840281266910 ) ) ;
#20556 = VECTOR ( 'NONE', #994, 39.37007874015748143 ) ;
#20557 = CARTESIAN_POINT ( 'NONE',  ( -0.3125000000000000000, 1.913510623667739771E-17, 0.2827777777777810142 ) ) ;
#20558 = VERTEX_POINT ( 'NONE', #2951 ) ;
#20559 = CARTESIAN_POINT ( 'NONE',  ( -0.3613381517857143232, 0.09732142847388614015, -0.1174058825155741143 ) ) ;
#20560 = DIRECTION ( 'NONE',  ( -0.6414950336115150531, 0.5424408363369016550, 0.5424408363369075392 ) ) ;
#20561 = ORIENTED_EDGE ( 'NONE', *, *, #2467, .T. ) ;
#20562 = APPROVAL_DATE_TIME ( #14383, #2844 ) ;
#20563 = CARTESIAN_POINT ( 'NONE',  ( 0.1306872919485616846, 0.3155070326520292290, 0.3817361111111154948 ) ) ;
#20564 = CARTESIAN_POINT ( 'NONE',  ( 0.2819296736111110424, 5.050777777853643791, -0.1167790944451423396 ) ) ;
#20565 = CARTESIAN_POINT ( 'NONE',  ( -0.1167790944451423535, 3.766055555631421470, 0.2819296736111110979 ) ) ;
#20566 = APPLICATION_CONTEXT ( 'configuration controlled 3d designs of mechanical parts and assemblies' ) ;
#20567 = CARTESIAN_POINT ( 'NONE',  ( -2.266361716303445225E-16, 4.432722222374099630, -0.3119999999999999996 ) ) ;
#20568 = CARTESIAN_POINT ( 'NONE',  ( -0.09435543239135868454, 3.066692553488282957, 2.763260016782451700 ) ) ;
#20569 = AXIS2_PLACEMENT_3D ( 'NONE', #13737, #22636, #13380 ) ;
#20570 = CARTESIAN_POINT ( 'NONE',  ( 0.1144950937579611444, 0.2764156081756483641, 0.1265277777777799595 ) ) ;
#20571 = CARTESIAN_POINT ( 'NONE',  ( -0.1167790944451422702, 0.3999999999241333204, -0.2819296736111110979 ) ) ;
#20572 = CARTESIAN_POINT ( 'NONE',  ( 0.1954553509668046640, -0.1954553509668047195, 0.3383333333333371495 ) ) ;
#20573 = CARTESIAN_POINT ( 'NONE',  ( -0.1167790944451423535, 4.932722222298088433, 0.2819296736111110424 ) ) ;
#20574 = CARTESIAN_POINT ( 'NONE',  ( 0.08172087692283847016, 4.462815503623632551, 0.3038682820922922190 ) ) ;
#20575 = CARTESIAN_POINT ( 'NONE',  ( 0.2819296736111110424, 4.828555555631420582, -0.1167790944451423396 ) ) ;
#20576 = LINE ( 'NONE', #14862, #13045 ) ;
#20577 = CARTESIAN_POINT ( 'NONE',  ( 0.0007453629615518840784, 4.877146636198903984, -0.3119992385510536037 ) ) ;
#20578 = DIRECTION ( 'NONE',  ( 0.000000000000000000, 0.000000000000000000, -1.000000000000000000 ) ) ;
#20579 = CARTESIAN_POINT ( 'NONE',  ( 0.2688584691416451289, -0.07459580784769219430, 0.3902639665736167829 ) ) ;
#20580 = CARTESIAN_POINT ( 'NONE',  ( 5.731347020009612645E-17, 4.509111111111110404, 0.3119999999999999996 ) ) ;
#20581 = CARTESIAN_POINT ( 'NONE',  ( 5.178964085587577574E-17, 3.755638888964754951, 0.2819296736111110979 ) ) ;
#20582 = CARTESIAN_POINT ( 'NONE',  ( 0.2206173157302027676, 0.3374999998482670627, 0.2206173157302028787 ) ) ;
#20583 = CARTESIAN_POINT ( 'NONE',  ( 9.101228903679513089E-16, 0.2392857142857141850, 0.4000000000000000222 ) ) ;
#20584 = CARTESIAN_POINT ( 'NONE',  ( -0.1049254751525411922, 3.735256410060579846, 0.2938276733034849153 ) ) ;
#20585 = CARTESIAN_POINT ( 'NONE',  ( 0.3111759409473714988, 4.584880126860398697, 0.02273571722973519171 ) ) ;
#20586 = ORIENTED_EDGE ( 'NONE', *, *, #15134, .T. ) ;
#20587 = B_SPLINE_CURVE_WITH_KNOTS ( 'NONE', 3,
 ( #12991, #11145, #1630, #1747 ),
 .UNSPECIFIED., .F., .F.,
 ( 4, 4 ),
 ( 0.02048720093474762707, 0.02195606945063139845 ),
 .UNSPECIFIED. ) ;
#20588 = DIRECTION ( 'NONE',  ( 0.000000000000000000, 0.000000000000000000, -1.000000000000000000 ) ) ;
#20589 = AXIS2_PLACEMENT_3D ( 'NONE', #10856, #18284, #12698 ) ;
#20590 = CARTESIAN_POINT ( 'NONE',  ( 0.1306872919485616846, 0.3155070326520292290, -0.1182638888888884604 ) ) ;
#20591 = LINE ( 'NONE', #11332, #19667 ) ;
#20592 = DIRECTION ( 'NONE',  ( -1.000000000000000000, 0.000000000000000000, 0.000000000000000000 ) ) ;
#20593 = VERTEX_POINT ( 'NONE', #5012 ) ;
#20594 = ADVANCED_FACE ( 'NONE', ( #6973 ), #3278, .T. ) ;
#20595 = CARTESIAN_POINT ( 'NONE',  ( -0.2923287055106771337, 0.3401785713310290227, 0.2123892367102619971 ) ) ;
#20596 = CARTESIAN_POINT ( 'NONE',  ( -0.1167790944451422702, 0.3305555554796889561, -0.2819296736111110424 ) ) ;
#20597 = CARTESIAN_POINT ( 'NONE',  ( 0.2209708691207961651, 0.2209708691207959985, 0.1577777777777804313 ) ) ;
#20598 = CARTESIAN_POINT ( 'NONE',  ( 0.000000000000000000, 3.700000000000000622, 0.3525000000000007017 ) ) ;
#20599 = CARTESIAN_POINT ( 'NONE',  ( 0.009374999999999772404, 0.5358532185916217161, 0.3779506566538943790 ) ) ;
#20600 = CARTESIAN_POINT ( 'NONE',  ( -0.1144950937579609779, 0.2764156081756484196, 0.2515277777777809587 ) ) ;
#20601 = ORIENTED_EDGE ( 'NONE', *, *, #24038, .T. ) ;
#20602 = CARTESIAN_POINT ( 'NONE',  ( -0.2691620460978288443, 5.100921413008813410, -0.1566095457824691894 ) ) ;
#20603 = CARTESIAN_POINT ( 'NONE',  ( -0.2206173157302028232, 4.710499999999999687, -0.2206173157302028232 ) ) ;
#20604 = CARTESIAN_POINT ( 'NONE',  ( -0.2206173157302028787, 0.1638888888888885287, 0.2206173157302027954 ) ) ;
#20605 = CARTESIAN_POINT ( 'NONE',  ( 0.3646812958242482416, 3.728225405753418098, -0.06420867857498598064 ) ) ;
#20606 = VECTOR ( 'NONE', #19459, 39.37007874015748143 ) ;
#20607 = EDGE_CURVE ( 'NONE', #175, #8540, #17951, .T. ) ;
#20608 = CARTESIAN_POINT ( 'NONE',  ( 0.2819296736111110424, 4.231333333409199149, -0.1167790944451423396 ) ) ;
#20609 = CARTESIAN_POINT ( 'NONE',  ( 0.3119999999999999996, 0.1256944442927115102, -0.1292346314604056468 ) ) ;
#20610 = DIRECTION ( 'NONE',  ( 0.7071067811865435759, 0.000000000000000000, 0.7071067811865514585 ) ) ;
#20611 = ORIENTED_EDGE ( 'NONE', *, *, #15835, .F. ) ;
#20612 = CARTESIAN_POINT ( 'NONE',  ( -0.2209708691207961373, -0.2209708691207961095, 0.1300000000000023914 ) ) ;
#20613 = CARTESIAN_POINT ( 'NONE',  ( 0.2819296736111110979, 4.988277777853642903, 0.1167790944451422425 ) ) ;
#20614 = CARTESIAN_POINT ( 'NONE',  ( 0.1913604482712364940, 4.188439349523841670, 0.2497711034849461054 ) ) ;
#20615 = DIRECTION ( 'NONE',  ( -0.000000000000000000, -1.000000000000000000, -0.000000000000000000 ) ) ;
#20616 = CARTESIAN_POINT ( 'NONE',  ( 0.2980062158858373667, -0.01674720435928796214, -0.08717288255250393858 ) ) ;
#20617 = CARTESIAN_POINT ( 'NONE',  ( 0.2819296736111110979, 4.602861111186975940, -3.452642723725051716E-17 ) ) ;
#20618 = DATE_AND_TIME ( #22447, #20496 ) ;
#20619 = CARTESIAN_POINT ( 'NONE',  ( 0.000000000000000000, 0.000000000000000000, 0.4425000000000000044 ) ) ;
#20620 = DIRECTION ( 'NONE',  ( 0.000000000000000000, 0.000000000000000000, 1.000000000000000000 ) ) ;
#20621 = CARTESIAN_POINT ( 'NONE',  ( 0.2819296736111110424, 0.5458333332574666352, 0.1167790944451424923 ) ) ;
#20622 = ORIENTED_EDGE ( 'NONE', *, *, #8548, .T. ) ;
#20623 = CARTESIAN_POINT ( 'NONE',  ( 0.2819296736111110424, 0.3236111110352444253, 0.1167790944451424923 ) ) ;
#20624 = CYLINDRICAL_SURFACE ( 'NONE', #11977, 0.3119999999999999996 ) ;
#20625 = EDGE_CURVE ( 'NONE', #20092, #7867, #1484, .T. ) ;
#20626 = LINE ( 'NONE', #9291, #19481 ) ;
#20627 = CARTESIAN_POINT ( 'NONE',  ( 0.3999999999999999667, 0.1892857142857141961, -0.1299678784931625475 ) ) ;
#20628 = CARTESIAN_POINT ( 'NONE',  ( -0.3155070326520293400, -0.1306872919485614626, -0.04534722222222162258 ) ) ;
#20629 = CARTESIAN_POINT ( 'NONE',  ( -0.3125000000000010547, -0.1294417382415911644, 0.01541666666666811208 ) ) ;
#20630 = DIRECTION ( 'NONE',  ( -0.000000000000000000, -1.000000000000000000, -0.000000000000000000 ) ) ;
#20631 = CARTESIAN_POINT ( 'NONE',  ( -0.2819296736111111534, 0.1777777777019111938, 0.1167790944451422563 ) ) ;
#20632 = CARTESIAN_POINT ( 'NONE',  ( 0.2819296736111110424, 0.09444444436857780956, -0.1167790944451423119 ) ) ;
#20633 = CARTESIAN_POINT ( 'NONE',  ( -0.2819296736111110979, 4.200083333409199149, 0.000000000000000000 ) ) ;
#20634 = CARTESIAN_POINT ( 'NONE',  ( -0.1236067977499790416, 0.08392857123348664017, 0.3804226065180614236 ) ) ;
#20635 = EDGE_CURVE ( 'NONE', #12983, #18582, #9977, .T. ) ;
#20636 = CARTESIAN_POINT ( 'NONE',  ( 0.2819296736111110424, 4.953555555631421470, -0.1167790944451423396 ) ) ;
#20637 = CARTESIAN_POINT ( 'NONE',  ( 0.1993543840281266633, 4.554250000075866112, -0.1993543840281266910 ) ) ;
#20638 = DIRECTION ( 'NONE',  ( -0.5000000000000003331, 0.000000000000000000, 0.8660254037844384856 ) ) ;
#20639 = AXIS2_PLACEMENT_3D ( 'NONE', #15813, #13878, #23473 ) ;
#20640 = ORIENTED_EDGE ( 'NONE', *, *, #14238, .F. ) ;
#20641 = CARTESIAN_POINT ( 'NONE',  ( -0.3125000000000000000, 1.913510623667739771E-17, 0.1161111111111130384 ) ) ;
#20642 = CARTESIAN_POINT ( 'NONE',  ( -0.2206173157302028232, 4.161888889040620931, -0.2206173157302028232 ) ) ;
#20643 = CARTESIAN_POINT ( 'NONE',  ( -0.2472135954999579999, 0.2946428569477723136, 0.3402603233408160732 ) ) ;
#20644 = LINE ( 'NONE', #2242, #21210 ) ;
#20645 = ORIENTED_EDGE ( 'NONE', *, *, #8863, .F. ) ;
#20646 = EDGE_CURVE ( 'NONE', #10582, #3466, #3669, .T. ) ;
#20647 = DATE_AND_TIME ( #5774, #2191 ) ;
#20648 = AXIS2_PLACEMENT_3D ( 'NONE', #10088, #2754, #10569 ) ;
#20649 = CARTESIAN_POINT ( 'NONE',  ( 0.000000000000000000, 0.06249999999999967387, 0.3119999999999999996 ) ) ;
#20650 = EDGE_CURVE ( 'NONE', #10641, #2833, #20855, .T. ) ;
#20651 = CARTESIAN_POINT ( 'NONE',  ( 0.3125000000000000000, 3.827021247335477694E-17, 1.326383476483184332 ) ) ;
#20652 = ORIENTED_EDGE ( 'NONE', *, *, #23118, .T. ) ;
#20653 = CARTESIAN_POINT ( 'NONE',  ( -0.3119999999999999996, 0.5388888887371559022, -3.820898013339742174E-17 ) ) ;
#20654 = EDGE_CURVE ( 'NONE', #18346, #17046, #21958, .T. ) ;
#20655 = VECTOR ( 'NONE', #11860, 39.37007874015748143 ) ;
#20656 = EDGE_CURVE ( 'NONE', #24096, #18008, #7569, .T. ) ;
#20657 = DIRECTION ( 'NONE',  ( 0.000000000000000000, 0.000000000000000000, -1.000000000000000000 ) ) ;
#20658 = CARTESIAN_POINT ( 'NONE',  ( 2.986000000000000210, 0.05000000000000028727, -0.07500000000000014988 ) ) ;
#20659 = CARTESIAN_POINT ( 'NONE',  ( -0.2923287055106771337, 0.09374999990245758141, -0.2123892367102620804 ) ) ;
#20660 = DIRECTION ( 'NONE',  ( 0.000000000000000000, -1.000000000000000000, 0.000000000000000000 ) ) ;
#20661 = ORIENTED_EDGE ( 'NONE', *, *, #8461, .T. ) ;
#20662 = CARTESIAN_POINT ( 'NONE',  ( -0.1116596296178200276, 0.1330357141881718663, 0.3436530038418508792 ) ) ;
#20663 = ORIENTED_EDGE ( 'NONE', *, *, #8582, .T. ) ;
#20664 = DIRECTION ( 'NONE',  ( -1.000000000000000000, 0.000000000000000000, 0.000000000000000000 ) ) ;
#20665 = CARTESIAN_POINT ( 'NONE',  ( -0.1292346314604106428, 4.061194444444443441, 0.3119999999999950036 ) ) ;
#20666 = EDGE_CURVE ( 'NONE', #7496, #16468, #9344, .T. ) ;
#20667 = CARTESIAN_POINT ( 'NONE',  ( -0.1167790944451423257, 4.064666666742532186, -0.2819296736111110424 ) ) ;
#20668 =( BOUNDED_SURFACE ( )  B_SPLINE_SURFACE ( 1, 2, ( 
 ( #5838, #15353, #6194, #19366, #20836, #2310, #9625, #2664, #22782, #11460, #6076, #10114, #4128, #18893, #2194, #351, #6799, #6552, #14002, #10229, #17776, #8373, #23124, #1069, #2892, #14120, #21549, #10470, #1194, #21435, #3023, #4960, #8500, #23483, #21675, #10589, #3140, #15824, #4720, #10352, #6922, #14240, #17899, #10705, #23243, #18140, #14360, #8738, #6675, #6435, #12547, #17656, #15940, #3254, #18016, #19483, #8626, #12427, #12193, #4840, #16071, #19840, #19720, #1314, #16194, #23608, #12306, #13889, #23366, #1437, #21790, #5079, #19967, #15710, #21317, #19599, #4607, #12069, #2776, #943, #16673, #18743, #23723, #3747, #24098, #7165, #18377, #10831, #1672, #11068, #11310, #3378, #23845, #18497, #5450, #3500, #7048, #3869, #20212, #10950, #12793, #1791, #14858, #23976, #9104, #16435, #9234, #7407, #22394, #8869, #7286, #12669, #14484, #22275, #20329, #14608, #16554, #9357, #5570, #13035, #20451, #80, #3618, #14972, #12918, #14738, #22153, #5695, #21908, #11191, #7525, #13158, #16799, #16310, #18620, #1912, #22031, #5198, #20572, #5328, #20089, #18259, #1554, #8992, #6292, #13274, #6168, #9599, #18864, #13631, #4459, #20930, #2038, #19099, #22757, #17394, #9964, #11559, #9845, #6048, #687, #11433, #22987, #9477, #8111, #15450, #7646, #5810, #13515, #7877, #561, #11676, #15565, #7998, #21170, #13745, #18986, #5928, #2286 ),
 ( #15208, #2405, #17276, #13388, #4223, #20811, #11923, #22873, #17156, #16910, #17031, #15327, #21049, #22517, #205, #2522, #446, #4339, #22643, #11790, #9720, #15094, #19215, #20691, #3982, #2166, #325, #7764, #4100, #23221, #16049, #6530, #921, #2867, #14098, #17877, #13982, #21410, #14217, #23462, #23102, #17631, #21771, #6411, #8718, #14339, #19824, #19343, #3002, #6773, #19457, #4699, #1169, #21653, #12166, #1048, #19574, #12284, #8351, #17509, #10327, #15803, #17753, #8475, #15916, #13863, #23583, #21291, #4941, #2755, #12044, #12405, #5058, #21525, #2640, #19699, #23338, #10570, #3119, #6652, #10451, #4815, #18000, #4584, #16168, #10089, #1292, #8608, #805, #10207, #6900, #8233, #15686, #22128, #18599, #11046, #7500, #9333, #5308, #16416, #22010, #18118, #1415, #7383, #11171, #18357, #23703, #1535, #5429, #12895, #23825, #23953, #7146, #14946, #16534, #3478, #54, #3356, #1650, #14834, #8843, #3724, #13012, #10928, #16653, #8967, #18475, #12771, #16290, #20189, #7267, #20310, #1769, #1890, #16770, #10809, #14587, #9214, #9084, #18237, #14715, #3595, #24074, #22251, #5547, #20427, #22368, #7024, #12528, #19947, #14467, #3233, #10684, #21891, #5180, #12650, #20069, #5787, #15183, #11651, #17252, #22620, #11529, #19075, #17134, #3961, #13363, #6141, #2383, #4197, #13489, #21023, #421, #11770, #2260, #5905, #17006, #2499, #20548 ) ),
 .UNSPECIFIED., .F., .F., .T. ) 
 B_SPLINE_SURFACE_WITH_KNOTS ( ( 2, 2 ),
 ( 3, 2, 2, 2, 2, 2, 2, 2, 2, 2, 2, 2, 2, 2, 2, 2, 2, 2, 2, 2, 2, 2, 2, 2, 2, 2, 2, 2, 2, 2, 2, 2, 2, 2, 2, 2, 2, 2, 2, 2, 2, 2, 2, 2, 2, 2, 2, 2, 2, 2, 2, 2, 2, 2, 2, 2, 2, 2, 2, 2, 2, 2, 2, 2, 2, 2, 2, 2, 2, 2, 2, 2, 2, 2, 2, 2, 2, 2, 2, 2, 2, 2, 2, 2, 2, 2, 2, 2, 2, 3 ),
 ( 0.000000000000000000, 1.000000000000000000 ),
 ( 0.000000000000000000, 0.01041666666666666609, 0.02083333333333333218, 0.03125000000000000000, 0.04166666666666666435, 0.05208333333333333565, 0.06250000000000000000, 0.07291666666666667129, 0.08333333333333332871, 0.09375000000000000000, 0.1041666666666666713, 0.1145833333333333287, 0.1250000000000000000, 0.1354166666666666574, 0.1458333333333333426, 0.1562500000000000000, 0.1666666666666666574, 0.1770833333333333426, 0.1875000000000000000, 0.1979166666666666574, 0.2083333333333333426, 0.2187500000000000000, 0.2291666666666666574, 0.2395833333333333426, 0.2500000000000000000, 0.2604166666666666852, 0.2708333333333333148, 0.2812500000000000000, 0.2916666666666666852, 0.3020833333333333148, 0.3125000000000000000, 0.3229166666666666852, 0.3333333333333333148, 0.3437500000000000000, 0.3541666666666666852, 0.3645833333333333148, 0.3750000000000000000, 0.3854166666666666852, 0.3958333333333333148, 0.4062500000000000000, 0.4166666666666666852, 0.4270833333333333148, 0.4375000000000000000, 0.4479166666666666852, 0.4583333333333333148, 0.4687500000000000000, 0.4791666666666666852, 0.4895833333333333148, 0.5000000000000000000, 0.5104166666666666297, 0.5208333333333333703, 0.5312500000000000000, 0.5416666666666666297, 0.5520833333333333703, 0.5625000000000000000, 0.5729166666666666297, 0.5833333333333333703, 0.5937500000000000000, 0.6041666666666666297, 0.6145833333333333703, 0.6250000000000000000, 0.6354166666666666297, 0.6458333333333333703, 0.6562500000000000000, 0.6666666666666666297, 0.6770833333333333703, 0.6875000000000000000, 0.6979166666666666297, 0.7083333333333333703, 0.7187500000000000000, 0.7291666666666666297, 0.7395833333333333703, 0.7500000000000000000, 0.7604166666666666297, 0.7708333333333333703, 0.7812500000000000000, 0.7916666666666666297, 0.8020833333333333703, 0.8125000000000000000, 0.8229166666666666297, 0.8333333333333333703, 0.8437500000000000000, 0.8541666666666666297, 0.8645833333333333703, 0.8750000000000000000, 0.8854166666666666297, 0.8958333333333333703, 0.9062500000000000000, 0.9166666666666666297, 0.9270833333333333703 ),
 .UNSPECIFIED. ) 
 GEOMETRIC_REPRESENTATION_ITEM ( )  RATIONAL_B_SPLINE_SURFACE ( (
 ( 1.000000000000000000, 0.9238795325112867385, 1.000000000000000000, 0.9238795325112867385, 1.000000000000000000, 0.9238795325112867385, 1.000000000000000000, 0.9238795325112867385, 1.000000000000000000, 0.9238795325112867385, 1.000000000000000000, 0.9238795325112867385, 1.000000000000000000, 0.9238795325112867385, 1.000000000000000000, 0.9238795325112867385, 1.000000000000000000, 0.9238795325112867385, 1.000000000000000000, 0.9238795325112867385, 1.000000000000000000, 0.9238795325112867385, 1.000000000000000000, 0.9238795325112867385, 1.000000000000000000, 0.9238795325112867385, 1.000000000000000000, 0.9238795325112867385, 1.000000000000000000, 0.9238795325112867385, 1.000000000000000000, 0.9238795325112867385, 1.000000000000000000, 0.9238795325112867385, 1.000000000000000000, 0.9238795325112867385, 1.000000000000000000, 0.9238795325112867385, 1.000000000000000000, 0.9238795325112867385, 1.000000000000000000, 0.9238795325112867385, 1.000000000000000000, 0.9238795325112867385, 1.000000000000000000, 0.9238795325112867385, 1.000000000000000000, 0.9238795325112867385, 1.000000000000000000, 0.9238795325112867385, 1.000000000000000000, 0.9238795325112867385, 1.000000000000000000, 0.9238795325112867385, 1.000000000000000000, 0.9238795325112867385, 1.000000000000000000, 0.9238795325112867385, 1.000000000000000000, 0.9238795325112867385, 1.000000000000000000, 0.9238795325112867385, 1.000000000000000000, 0.9238795325112867385, 1.000000000000000000, 0.9238795325112867385, 1.000000000000000000, 0.9238795325112867385, 1.000000000000000000, 0.9238795325112867385, 1.000000000000000000, 0.9238795325112867385, 1.000000000000000000, 0.9238795325112867385, 1.000000000000000000, 0.9238795325112867385, 1.000000000000000000, 0.9238795325112867385, 1.000000000000000000, 0.9238795325112867385, 1.000000000000000000, 0.9238795325112867385, 1.000000000000000000, 0.9238795325112867385, 1.000000000000000000, 0.9238795325112867385, 1.000000000000000000, 0.9238795325112867385, 1.000000000000000000, 0.9238795325112867385, 1.000000000000000000, 0.9238795325112867385, 1.000000000000000000, 0.9238795325112867385, 1.000000000000000000, 0.9238795325112867385, 1.000000000000000000, 0.9238795325112867385, 1.000000000000000000, 0.9238795325112867385, 1.000000000000000000, 0.9238795325112867385, 1.000000000000000000, 0.9238795325112867385, 1.000000000000000000, 0.9238795325112867385, 1.000000000000000000, 0.9238795325112867385, 1.000000000000000000, 0.9238795325112867385, 1.000000000000000000, 0.9238795325112867385, 1.000000000000000000, 0.9238795325112867385, 1.000000000000000000, 0.9238795325112867385, 1.000000000000000000, 0.9238795325112867385, 1.000000000000000000, 0.9238795325112867385, 1.000000000000000000, 0.9238795325112867385, 1.000000000000000000, 0.9238795325112867385, 1.000000000000000000, 0.9238795325112867385, 1.000000000000000000, 0.9238795325112867385, 1.000000000000000000, 0.9238795325112867385, 1.000000000000000000, 0.9238795325112867385, 1.000000000000000000, 0.9238795325112867385, 1.000000000000000000, 0.9238795325112867385, 1.000000000000000000, 0.9238795325112867385, 1.000000000000000000, 0.9238795325112867385, 1.000000000000000000, 0.9238795325112867385, 1.000000000000000000, 0.9238795325112867385, 1.000000000000000000, 0.9238795325112867385, 1.000000000000000000, 0.9238795325112867385, 1.000000000000000000, 0.9238795325112867385, 1.000000000000000000, 0.9238795325112867385, 1.000000000000000000, 0.9238795325112867385, 1.000000000000000000, 0.9238795325112867385, 1.000000000000000000, 0.9238795325112867385, 1.000000000000000000, 0.9238795325112867385, 1.000000000000000000, 0.9238795325112867385, 1.000000000000000000, 0.9238795325112867385, 1.000000000000000000, 0.9238795325112867385, 1.000000000000000000, 0.9238795325112867385, 1.000000000000000000, 0.9238795325112867385, 1.000000000000000000, 0.9238795325112867385, 1.000000000000000000, 0.9238795325112867385, 1.000000000000000000, 0.9238795325112867385, 1.000000000000000000, 0.9238795325112867385, 1.000000000000000000),
 ( 1.000000000000000000, 0.9238795325112867385, 1.000000000000000000, 0.9238795325112867385, 1.000000000000000000, 0.9238795325112867385, 1.000000000000000000, 0.9238795325112867385, 1.000000000000000000, 0.9238795325112867385, 1.000000000000000000, 0.9238795325112867385, 1.000000000000000000, 0.9238795325112867385, 1.000000000000000000, 0.9238795325112867385, 1.000000000000000000, 0.9238795325112867385, 1.000000000000000000, 0.9238795325112867385, 1.000000000000000000, 0.9238795325112867385, 1.000000000000000000, 0.9238795325112867385, 1.000000000000000000, 0.9238795325112867385, 1.000000000000000000, 0.9238795325112867385, 1.000000000000000000, 0.9238795325112867385, 1.000000000000000000, 0.9238795325112867385, 1.000000000000000000, 0.9238795325112867385, 1.000000000000000000, 0.9238795325112867385, 1.000000000000000000, 0.9238795325112867385, 1.000000000000000000, 0.9238795325112867385, 1.000000000000000000, 0.9238795325112867385, 1.000000000000000000, 0.9238795325112867385, 1.000000000000000000, 0.9238795325112867385, 1.000000000000000000, 0.9238795325112867385, 1.000000000000000000, 0.9238795325112867385, 1.000000000000000000, 0.9238795325112867385, 1.000000000000000000, 0.9238795325112867385, 1.000000000000000000, 0.9238795325112867385, 1.000000000000000000, 0.9238795325112867385, 1.000000000000000000, 0.9238795325112867385, 1.000000000000000000, 0.9238795325112867385, 1.000000000000000000, 0.9238795325112867385, 1.000000000000000000, 0.9238795325112867385, 1.000000000000000000, 0.9238795325112867385, 1.000000000000000000, 0.9238795325112867385, 1.000000000000000000, 0.9238795325112867385, 1.000000000000000000, 0.9238795325112867385, 1.000000000000000000, 0.9238795325112867385, 1.000000000000000000, 0.9238795325112867385, 1.000000000000000000, 0.9238795325112867385, 1.000000000000000000, 0.9238795325112867385, 1.000000000000000000, 0.9238795325112867385, 1.000000000000000000, 0.9238795325112867385, 1.000000000000000000, 0.9238795325112867385, 1.000000000000000000, 0.9238795325112867385, 1.000000000000000000, 0.9238795325112867385, 1.000000000000000000, 0.9238795325112867385, 1.000000000000000000, 0.9238795325112867385, 1.000000000000000000, 0.9238795325112867385, 1.000000000000000000, 0.9238795325112867385, 1.000000000000000000, 0.9238795325112867385, 1.000000000000000000, 0.9238795325112867385, 1.000000000000000000, 0.9238795325112867385, 1.000000000000000000, 0.9238795325112867385, 1.000000000000000000, 0.9238795325112867385, 1.000000000000000000, 0.9238795325112867385, 1.000000000000000000, 0.9238795325112867385, 1.000000000000000000, 0.9238795325112867385, 1.000000000000000000, 0.9238795325112867385, 1.000000000000000000, 0.9238795325112867385, 1.000000000000000000, 0.9238795325112867385, 1.000000000000000000, 0.9238795325112867385, 1.000000000000000000, 0.9238795325112867385, 1.000000000000000000, 0.9238795325112867385, 1.000000000000000000, 0.9238795325112867385, 1.000000000000000000, 0.9238795325112867385, 1.000000000000000000, 0.9238795325112867385, 1.000000000000000000, 0.9238795325112867385, 1.000000000000000000, 0.9238795325112867385, 1.000000000000000000, 0.9238795325112867385, 1.000000000000000000, 0.9238795325112867385, 1.000000000000000000, 0.9238795325112867385, 1.000000000000000000, 0.9238795325112867385, 1.000000000000000000, 0.9238795325112867385, 1.000000000000000000, 0.9238795325112867385, 1.000000000000000000, 0.9238795325112867385, 1.000000000000000000, 0.9238795325112867385, 1.000000000000000000, 0.9238795325112867385, 1.000000000000000000, 0.9238795325112867385, 1.000000000000000000, 0.9238795325112867385, 1.000000000000000000, 0.9238795325112867385, 1.000000000000000000, 0.9238795325112867385, 1.000000000000000000, 0.9238795325112867385, 1.000000000000000000, 0.9238795325112867385, 1.000000000000000000, 0.9238795325112867385, 1.000000000000000000, 0.9238795325112867385, 1.000000000000000000, 0.9238795325112867385, 1.000000000000000000, 0.9238795325112867385, 1.000000000000000000, 0.9238795325112867385, 1.000000000000000000) ) ) 
 REPRESENTATION_ITEM ( '' )  SURFACE ( )  );
#20669 =( BOUNDED_CURVE ( )  B_SPLINE_CURVE ( 2, ( #13859, #9960, #10084, #19571, #2518, #4455, #4581, #9840, #13627 ),
 .UNSPECIFIED., .F., .F. ) 
 B_SPLINE_CURVE_WITH_KNOTS ( ( 3, 2, 2, 2, 3 ),
 ( 0.2395833333333334259, 0.2500000000000000555, 0.2604166666666667962, 0.2708333333333334259, 0.2812500000000000555 ),
 .UNSPECIFIED. ) 
 CURVE ( )  GEOMETRIC_REPRESENTATION_ITEM ( )  RATIONAL_B_SPLINE_CURVE ( ( 0.9999999999999995559, 0.9238795325112871826, 1.000000000000000000, 0.9238795325112867385, 1.000000000000000000, 0.9238795325112867385, 1.000000000000000000, 0.9238795325112862944, 1.000000000000000444 ) ) 
 REPRESENTATION_ITEM ( '' )  );
#20670 = CARTESIAN_POINT ( 'NONE',  ( 0.1129719973630488317, 5.040650656955687481, -0.2914126276313158126 ) ) ;
#20671 = CARTESIAN_POINT ( 'NONE',  ( 0.4223122635727384888, -0.2974437783094736054, 0.07051021533369883354 ) ) ;
#20672 = CARTESIAN_POINT ( 'NONE',  ( 0.1292346314604058410, 3.790361111111110404, 0.3119999999999998885 ) ) ;
#20673 = CARTESIAN_POINT ( 'NONE',  ( -0.2206173157302027676, 4.675777777929510215, 0.2206173157302028787 ) ) ;
#20674 = CARTESIAN_POINT ( 'NONE',  ( -0.1167790944451423535, 5.099388888964754507, 0.2819296736111110979 ) ) ;
#20675 = VECTOR ( 'NONE', #10243, 39.37007874015748143 ) ;
#20676 = CARTESIAN_POINT ( 'NONE',  ( -0.1993543840281266910, 4.345916666742532186, -0.1993543840281266910 ) ) ;
#20677 = CARTESIAN_POINT ( 'NONE',  ( -0.1274622673633111769, 3.901219489371187343, 0.2865353922227728556 ) ) ;
#20678 = VERTEX_POINT ( 'NONE', #20377 ) ;
#20679 = CARTESIAN_POINT ( 'NONE',  ( -0.3613381517857143232, 0.1008928570453147405, -4.425116109941954795E-17 ) ) ;
#20680 = ORIENTED_EDGE ( 'NONE', *, *, #16450, .T. ) ;
#20681 = ORIENTED_EDGE ( 'NONE', *, *, #2888, .T. ) ;
#20682 = COORDINATED_UNIVERSAL_TIME_OFFSET ( 0, 0, .AHEAD. ) ;
#20683 = DIRECTION ( 'NONE',  ( -1.000000000000000000, 0.000000000000000000, 0.000000000000000000 ) ) ;
#20684 = CARTESIAN_POINT ( 'NONE',  ( 0.1993543840281266633, 5.165361111186976828, -0.1993543840281266910 ) ) ;
#20685 = CARTESIAN_POINT ( 'NONE',  ( 0.2819296736111110979, 3.786888888964754507, -0.1167790944451423396 ) ) ;
#20686 = LINE ( 'NONE', #11428, #6842 ) ;
#20687 = CARTESIAN_POINT ( 'NONE',  ( 0.4593750000000004219, -0.2760455974562899262, 0.06112444011295369711 ) ) ;
#20688 = VECTOR ( 'NONE', #22611, 39.37007874015748143 ) ;
#20689 = CARTESIAN_POINT ( 'NONE',  ( -3.385114897866767815E-17, -0.2764156081756484196, 0.1577777777777801815 ) ) ;
#20690 = CARTESIAN_POINT ( 'NONE',  ( -0.1993543840281266633, 0.5145833332574666352, -0.1993543840281266910 ) ) ;
#20691 = CARTESIAN_POINT ( 'NONE',  ( -0.1144950937579609918, -0.2764156081756484196, -0.06791666666666602847 ) ) ;
#20692 = ADVANCED_FACE ( 'NONE', ( #16603 ), #21218, .T. ) ;
#20693 = CARTESIAN_POINT ( 'NONE',  ( 0.1993543840281267465, 4.998694444520309865, 0.1993543840281266633 ) ) ;
#20694 = CARTESIAN_POINT ( 'NONE',  ( -0.01298578716746940157, -0.5473886244374777110, 0.04271891838948295439 ) ) ;
#20695 = EDGE_CURVE ( 'NONE', #6543, #8220, #20733, .T. ) ;
#20696 = CARTESIAN_POINT ( 'NONE',  ( -0.1993543840281266910, 4.901472222298087544, -0.1993543840281266910 ) ) ;
#20697 = CARTESIAN_POINT ( 'NONE',  ( -0.08067706695034009001, 4.180438756533890299, 0.3020759868123111813 ) ) ;
#20698 = CARTESIAN_POINT ( 'NONE',  ( 0.1567781121482516860, 4.854100146818556283, 0.2702798039214149295 ) ) ;
#20699 = CARTESIAN_POINT ( 'NONE',  ( 5.731347020009612645E-17, 4.175777777777776478, 0.3119999999999999996 ) ) ;
#20700 = FACE_OUTER_BOUND ( 'NONE', #17070, .T. ) ;
#20701 = CARTESIAN_POINT ( 'NONE',  ( 0.3119999999999999996, 4.411888888888888083, -3.820898013339742174E-17 ) ) ;
#20702 = CARTESIAN_POINT ( 'NONE',  ( -0.2819296736111110979, 3.741750000075865668, 0.000000000000000000 ) ) ;
#20703 = CARTESIAN_POINT ( 'NONE',  ( -0.1292346314604032043, 4.207027777777776478, -0.3120000000000024420 ) ) ;
#20704 = CARTESIAN_POINT ( 'NONE',  ( -0.3236067977499790249, 0.2285714285714285088, 0.2351141009169892271 ) ) ;
#20705 = CARTESIAN_POINT ( 'NONE',  ( 0.5097595264191659981, 2.291712385858714729, -0.6667552972947653478 ) ) ;
#20706 = ORIENTED_EDGE ( 'NONE', *, *, #2030, .F. ) ;
#20707 = CARTESIAN_POINT ( 'NONE',  ( -0.3108513798347909418, -0.3617957495396915135, 0.4142710792078265203 ) ) ;
#20708 = CYLINDRICAL_SURFACE ( 'NONE', #17003, 0.7500000000000001110 ) ;
#20709 = CARTESIAN_POINT ( 'NONE',  ( 0.3155070326520292290, -0.1306872919485616569, -0.07659722222222146992 ) ) ;
#20710 = CARTESIAN_POINT ( 'NONE',  ( -0.2726212802448290673, 3.941984754839822802, -0.1571292508600286020 ) ) ;
#20711 = CARTESIAN_POINT ( 'NONE',  ( 0.3033563106615940752, 5.146283422524257745, -0.006787276862509872624 ) ) ;
#20713 = VERTEX_POINT ( 'NONE', #851 ) ;
#20712 = CC_DESIGN_DATE_AND_TIME_ASSIGNMENT ( #23743, #6820, ( #9710 ) ) ;
#20714 = CARTESIAN_POINT ( 'NONE',  ( -0.3613381517857143232, 0.2580357141881718386, -0.1174058825155741004 ) ) ;
#20715 = CARTESIAN_POINT ( 'NONE',  ( -0.1993543840281266633, 0.5562499999241333759, -0.1993543840281266910 ) ) ;
#20716 = DIRECTION ( 'NONE',  ( 0.000000000000000000, 0.000000000000000000, 1.000000000000000000 ) ) ;
#20717 = CARTESIAN_POINT ( 'NONE',  ( 0.05168019678275902890, 0.1836979246868377935, -1.240975288036999080 ) ) ;
#20718 = CARTESIAN_POINT ( 'NONE',  ( -0.3119999999999999996, 0.1534722222222218990, -0.1292346314604056745 ) ) ;
#20719 = CARTESIAN_POINT ( 'NONE',  ( 0.2764156081756483641, 0.1144950937579610056, 0.2376388888888919526 ) ) ;
#20720 = CARTESIAN_POINT ( 'NONE',  ( -0.1166234456863257940, 1.999640111863030478, -2.868834514064774854 ) ) ;
#20721 = CARTESIAN_POINT ( 'NONE',  ( 0.2472135954999579166, 0.09464285694777231639, 0.3402603233408160732 ) ) ;
#20722 = CARTESIAN_POINT ( 'NONE',  ( 0.1292346314604057023, 0.3409722222222218435, 0.3119999999999998885 ) ) ;
#20723 = CARTESIAN_POINT ( 'NONE',  ( -0.2206173157302027676, 5.113277777777777366, 0.2206173157302028787 ) ) ;
#20724 = CARTESIAN_POINT ( 'NONE',  ( 5.178964085587577574E-17, 4.158416666742532186, 0.2819296736111110979 ) ) ;
#20725 = DIRECTION ( 'NONE',  ( -0.000000000000000000, -1.000000000000000000, -0.000000000000000000 ) ) ;
#20726 = CARTESIAN_POINT ( 'NONE',  ( -0.3616234456863257618, 4.559812086079793048, -2.727383698113316157 ) ) ;
#20727 = ORIENTED_EDGE ( 'NONE', *, *, #13818, .F. ) ;
#20728 = VERTEX_POINT ( 'NONE', #15614 ) ;
#20729 = CARTESIAN_POINT ( 'NONE',  ( 0.1294417382415921358, -0.3125000000000002220, 0.1404166666666691321 ) ) ;
#20730 = CARTESIAN_POINT ( 'NONE',  ( 0.1993543840281266633, 4.943138888964754507, -0.1993543840281266910 ) ) ;
#20731 = VECTOR ( 'NONE', #16916, 39.37007874015748143 ) ;
#20732 = EDGE_CURVE ( 'NONE', #3958, #20369, #5317, .T. ) ;
#20733 = B_SPLINE_CURVE_WITH_KNOTS ( 'NONE', 3,
 ( #2080, #15251, #1834, #4148, #24022, #22682, #5855, #22200, #11116, #7687, #22564, #11477, #18912, #5972, #2213, #14784, #5500, #9402, #18663, #16841, #12963, #9643, #17077, #18545, #368, #16720, #1425, #7450, #14897, #22317, #5617, #23033, #8396, #15847, #17679, #4738, #10015, #2684, #15492, #7920, #21095, #13562, #4507, #17559, #613 ),
 .UNSPECIFIED., .F., .F.,
 ( 4, 2, 2, 2, 2, 2, 2, 1, 2, 2, 2, 2, 2, 2, 2, 2, 2, 2, 2, 2, 2, 2, 4 ),
 ( 0.06676172314147620079, 0.06751374342960875241, 0.06826576371774129015, 0.06976980429400639339, 0.07127384487027149662, 0.07277788544653658598, 0.07352990573466913760, 0.07428192602280167534, 0.07503394631093422695, 0.07578596659906677857, 0.07729000717533186793, 0.07804202746346441955, 0.07879404775159697116, 0.08029808832786206052, 0.08105010861599461214, 0.08180212890412716376, 0.08330616948039225311, 0.08481021005665734247, 0.08556223034478989409, 0.08631425063292244571, 0.08781829120918754894, 0.08932233178545265218, 0.09082637236171775541 ),
 .UNSPECIFIED. ) ;
#20734 = CARTESIAN_POINT ( 'NONE',  ( 0.1568014993035689308, 4.187283761971905882, 0.2727961053911494571 ) ) ;
#20735 = EDGE_CURVE ( 'NONE', #6859, #13196, #22921, .T. ) ;
#20736 = DIRECTION ( 'NONE',  ( 1.000000000000000000, 0.000000000000000000, 0.000000000000000000 ) ) ;
#20737 = CARTESIAN_POINT ( 'NONE',  ( -0.2764156081756484196, 0.1144950937579609918, -0.1373611111111110172 ) ) ;
#20738 = CARTESIAN_POINT ( 'NONE',  ( 0.1993543840281266633, 4.401472222298088433, -0.1993543840281266910 ) ) ;
#20739 = DATE_TIME_ROLE ( 'classification_date' ) ;
#20740 = CC_DESIGN_DATE_AND_TIME_ASSIGNMENT ( #20618, #375, ( #3736 ) ) ;
#20741 = CARTESIAN_POINT ( 'NONE',  ( -1.910449006669871087E-17, 4.314666666666665762, -0.3119999999999999996 ) ) ;
#20742 = CARTESIAN_POINT ( 'NONE',  ( -0.2764156081756484196, -0.1144950937579609362, 0.04319444444444596465 ) ) ;
#20743 = CARTESIAN_POINT ( 'NONE',  ( 0.2819296736111110424, 0.6083333332574668573, -0.1167790944451423119 ) ) ;
#20744 = ORIENTED_EDGE ( 'NONE', *, *, #7522, .T. ) ;
#20745 = CARTESIAN_POINT ( 'NONE',  ( 0.1993543840281266355, 0.5423611110352445364, 0.1993543840281267465 ) ) ;
#20746 = CARTESIAN_POINT ( 'NONE',  ( 0.3120000000000000551, 4.130638888888888083, 0.1292346314604056190 ) ) ;
#20747 = CARTESIAN_POINT ( 'NONE',  ( -0.1236067977499790416, 0.3696428569477722137, 0.3804226065180614236 ) ) ;
#20748 = CARTESIAN_POINT ( 'NONE',  ( -0.3236067977499789694, 0.2142857142857142461, -0.2351141009169893104 ) ) ;
#20749 = CARTESIAN_POINT ( 'NONE',  ( -0.2230971623002954152, -0.2230971623002953874, 0.06923611111111260819 ) ) ;
#20750 = CIRCLE ( 'NONE', #12210, 0.2500000000000000000 ) ;
#20751 = CARTESIAN_POINT ( 'NONE',  ( 2.948500000000001009, 2.727500000000000924, -0.03750000000000084516 ) ) ;
#20752 = LINE ( 'NONE', #9788, #10140 ) ;
#20753 = CARTESIAN_POINT ( 'NONE',  ( -0.1993543840281267465, 0.2368055554796889561, 0.1993543840281266633 ) ) ;
#20754 = CARTESIAN_POINT ( 'NONE',  ( 0.2819296736111110424, 0.3166666665908000056, -0.1167790944451423119 ) ) ;
#20755 = ORIENTED_EDGE ( 'NONE', *, *, #13075, .T. ) ;
#20756 = CARTESIAN_POINT ( 'NONE',  ( -0.2819296736111110424, 4.307722222298088433, -0.1167790944451423119 ) ) ;
#20757 = CARTESIAN_POINT ( 'NONE',  ( -0.2472135954999579999, 0.008928571233486644679, 0.3402603233408159622 ) ) ;
#20758 = CARTESIAN_POINT ( 'NONE',  ( -0.1993543840281266910, 4.970916666742532186, -0.1993543840281266910 ) ) ;
#20759 = CARTESIAN_POINT ( 'NONE',  ( -0.1167790944451423535, 4.529944444520309865, 0.2819296736111110979 ) ) ;
#20760 = CARTESIAN_POINT ( 'NONE',  ( 0.2615470475763201352, 5.073407320188289660, 0.1707168293479552346 ) ) ;
#20761 = CARTESIAN_POINT ( 'NONE',  ( -8.964115882027956832E-07, 3.710500024236165206, -0.3119999999987121964 ) ) ;
#20762 = CARTESIAN_POINT ( 'NONE',  ( -0.3119999999999999996, 4.109805555707288782, -0.1292346314604056468 ) ) ;
#20763 = CARTESIAN_POINT ( 'NONE',  ( 0.7108475124358382136, 4.111524471938507119, -3.019372695974962717 ) ) ;
#20764 = EDGE_CURVE ( 'NONE', #1879, #2780, #19312, .T. ) ;
#20765 = VECTOR ( 'NONE', #21166, 39.37007874015748143 ) ;
#20766 = DIRECTION ( 'NONE',  ( 0.000000000000000000, 0.000000000000000000, -1.000000000000000000 ) ) ;
#20767 = ORIENTED_EDGE ( 'NONE', *, *, #19300, .T. ) ;
#20768 = APPROVAL_STATUS ( 'not_yet_approved' ) ;
#20769 = ADVANCED_FACE ( 'NONE', ( #732 ), #13788, .F. ) ;
#20770 = CARTESIAN_POINT ( 'NONE',  ( 0.1376066337087315239, 0.2509841804965753376, 0.3977425164349297493 ) ) ;
#20771 = DIRECTION ( 'NONE',  ( 0.000000000000000000, 0.000000000000000000, 1.000000000000000000 ) ) ;
#20772 = CARTESIAN_POINT ( 'NONE',  ( -0.04066036887665752664, 4.989443942244452757, -0.3119999862560016712 ) ) ;
#20773 = ORIENTED_EDGE ( 'NONE', *, *, #4005, .T. ) ;
#20774 = CARTESIAN_POINT ( 'NONE',  ( -0.2206173157302028787, 0.6013888887371559022, 0.2206173157302027954 ) ) ;
#20775 = CYLINDRICAL_SURFACE ( 'NONE', #20261, 0.3119999999999999996 ) ;
#20776 = CARTESIAN_POINT ( 'NONE',  ( 0.03677510111070102922, 0.5081344126854514531, 0.4062297518000476670 ) ) ;
#20777 = CARTESIAN_POINT ( 'NONE',  ( -3.345742422185251127E-06, 4.766055647721512578, -0.3119999999820609049 ) ) ;
#20778 = CARTESIAN_POINT ( 'NONE',  ( 0.3613381517857143232, 0.1330357141881718941, 0.1174058825155742114 ) ) ;
#20779 = CARTESIAN_POINT ( 'NONE',  ( 0.009615703107365407981, 5.190106621824546629, -0.2891886902264009795 ) ) ;
#20780 = ORIENTED_EDGE ( 'NONE', *, *, #1230, .T. ) ;
#20781 = CARTESIAN_POINT ( 'NONE',  ( 0.1116596296178199860, 0.3830357141881718386, -0.3436530038418508792 ) ) ;
#20782 = CARTESIAN_POINT ( 'NONE',  ( 0.3125000000000000000, -5.740531871003217465E-17, 0.08833333333333501236 ) ) ;
#20783 = CARTESIAN_POINT ( 'NONE',  ( -0.2228749573452438737, 4.675693542979938222, 0.2183525872440850724 ) ) ;
#20784 = AXIS2_PLACEMENT_3D ( 'NONE', #22305, #9267, #14886 ) ;
#20785 = CARTESIAN_POINT ( 'NONE',  ( 5.178964085587577574E-17, 4.033416666742532186, 0.2819296736111110979 ) ) ;
#20786 = LINE ( 'NONE', #540, #11030 ) ;
#20787 = CARTESIAN_POINT ( 'NONE',  ( -1.910449006669871087E-17, 4.814666666666665762, -0.3119999999999999996 ) ) ;
#20788 = CARTESIAN_POINT ( 'NONE',  ( -1.910449006669871087E-17, 3.925777777777776922, -0.3119999999999999996 ) ) ;
#20789 = CARTESIAN_POINT ( 'NONE',  ( 0.3119999999999999996, 4.755638889040620043, -0.1292346314604056745 ) ) ;
#20790 = CARTESIAN_POINT ( 'NONE',  ( -0.1993543840281266910, 4.859805555631421470, -0.1993543840281266910 ) ) ;
#20791 = EDGE_LOOP ( 'NONE', ( #9744, #21400, #3257, #19326 ) ) ;
#20792 = EDGE_CURVE ( 'NONE', #7614, #22384, #13909, .T. ) ;
#20793 = EDGE_CURVE ( 'NONE', #9670, #3584, #20436, .T. ) ;
#20794 = CARTESIAN_POINT ( 'NONE',  ( -0.1993543840281266355, 4.248694444520309865, 0.1993543840281267465 ) ) ;
#20795 = EDGE_CURVE ( 'NONE', #23206, #11776, #23633, .T. ) ;
#20796 = CARTESIAN_POINT ( 'NONE',  ( 0.1116596296178199860, 0.1508928570453147155, -0.3436530038418508792 ) ) ;
#20797 = ORIENTED_EDGE ( 'NONE', *, *, #16641, .F. ) ;
#20798 = ORIENTED_EDGE ( 'NONE', *, *, #8568, .F. ) ;
#20799 = PERSON_AND_ORGANIZATION_ROLE ( 'classification_officer' ) ;
#20800 = AXIS2_PLACEMENT_3D ( 'NONE', #12287, #23343, #4817 ) ;
#20801 = EDGE_CURVE ( 'NONE', #11465, #20410, #23385, .T. ) ;
#20802 = CARTESIAN_POINT ( 'NONE',  ( -0.1306872919485615459, -0.3155070326520293400, 0.4095138888888935069 ) ) ;
#20803 = DIRECTION ( 'NONE',  ( 0.000000000000000000, 1.000000000000000000, 0.000000000000000000 ) ) ;
#20804 = CARTESIAN_POINT ( 'NONE',  ( -0.2819296736111110979, 3.918833333409198705, -0.1167790944451422980 ) ) ;
#20805 = CARTESIAN_POINT ( 'NONE',  ( 0.02037670883466128138, 4.432138282695498255, -0.3119999999999997220 ) ) ;
#20806 = DIRECTION ( 'NONE',  ( -1.000000000000000000, -0.000000000000000000, -0.000000000000000000 ) ) ;
#20807 = CARTESIAN_POINT ( 'NONE',  ( 0.08337866210071723239, -0.4931271843567546220, 0.07807775719021840810 ) ) ;
#20808 = ORIENTED_EDGE ( 'NONE', *, *, #23240, .F. ) ;
#20809 = CARTESIAN_POINT ( 'NONE',  ( 0.2764156081756483641, 0.1144950937579610195, 0.1751388888888914530 ) ) ;
#20810 = CARTESIAN_POINT ( 'NONE',  ( 0.1167790944451423119, 0.3930555554796889561, -0.2819296736111110979 ) ) ;
#20811 = CARTESIAN_POINT ( 'NONE',  ( -0.2764156081756484196, -0.1144950937579609362, -0.1304166666666665420 ) ) ;
#20812 = CARTESIAN_POINT ( 'NONE',  ( 0.2819296736111110424, 4.953555555631421470, -0.1167790944451423396 ) ) ;
#20813 = CARTESIAN_POINT ( 'NONE',  ( 0.1918522775149521797, 4.466287634334791257, 0.2494131876992732866 ) ) ;
#20814 = CARTESIAN_POINT ( 'NONE',  ( -0.2819296736111110424, 4.634111111186976828, 0.1167790944451424923 ) ) ;
#20815 = CARTESIAN_POINT ( 'NONE',  ( -0.2437787738197921550, 0.1452258864492545765, -0.07229589000035700763 ) ) ;
#20816 = EDGE_CURVE ( 'NONE', #20864, #20538, #345, .T. ) ;
#20817 = CARTESIAN_POINT ( 'NONE',  ( 0.2903586046000930510, 4.866586313092618354, -0.1141781630894242727 ) ) ;
#20818 = CARTESIAN_POINT ( 'NONE',  ( -0.3583630266090071514, -7.597319298711557862E-17, 0.1657390341004710554 ) ) ;
#20819 = CARTESIAN_POINT ( 'NONE',  ( 2.159030003005114828, 2.291712385858714285, -2.568740473580834127 ) ) ;
#20820 = CARTESIAN_POINT ( 'NONE',  ( -1.910449006669871087E-17, 4.536888888888888083, -0.3119999999999999996 ) ) ;
#20821 = CARTESIAN_POINT ( 'NONE',  ( 2.356802308782948607, 2.740000000000000213, -2.515999999999999570 ) ) ;
#20822 = CIRCLE ( 'NONE', #14206, 0.01875000000000002359 ) ;
#20823 = CARTESIAN_POINT ( 'NONE',  ( -0.1292346314604057300, 4.227861111111110404, 0.3119999999999998885 ) ) ;
#20824 = ORIENTED_EDGE ( 'NONE', *, *, #15576, .F. ) ;
#20825 = CARTESIAN_POINT ( 'NONE',  ( 0.3108980883051527533, 4.584783822353920790, 0.02619940625674591766 ) ) ;
#20826 = ORIENTED_EDGE ( 'NONE', *, *, #22035, .T. ) ;
#20827 =( GEOMETRIC_REPRESENTATION_CONTEXT ( 3 ) GLOBAL_UNCERTAINTY_ASSIGNED_CONTEXT ( ( #15583 ) ) GLOBAL_UNIT_ASSIGNED_CONTEXT ( ( #5744, #128, #18785 ) ) REPRESENTATION_CONTEXT ( 'NONE', 'WORKASPACE' ) );
#20828 = CARTESIAN_POINT ( 'NONE',  ( 0.0003785305096514256316, 4.710489828778345434, -0.3119998034525927055 ) ) ;
#20829 = CARTESIAN_POINT ( 'NONE',  ( 0.09510778779462622512, 4.652184472055949094, -0.2980982098042628814 ) ) ;
#20830 = CARTESIAN_POINT ( 'NONE',  ( 0.3155070326520292290, -0.1306872919485616569, -0.1321527777777774804 ) ) ;
#20831 = VECTOR ( 'NONE', #11580, 39.37007874015748143 ) ;
#20832 = DIRECTION ( 'NONE',  ( -0.000000000000000000, -1.000000000000000000, -0.000000000000000000 ) ) ;
#20833 = VERTEX_POINT ( 'NONE', #12444 ) ;
#20834 = CARTESIAN_POINT ( 'NONE',  ( 0.3613381517857143232, 0.06517857133102902822, 0.000000000000000000 ) ) ;
#20835 = CARTESIAN_POINT ( 'NONE',  ( -0.1993543840281266633, 0.5006944443685777957, -0.1993543840281266910 ) ) ;
#20836 = CARTESIAN_POINT ( 'NONE',  ( -0.2764156081756484196, 1.692557448933383907E-17, -0.1269444444444443043 ) ) ;
#20837 = CARTESIAN_POINT ( 'NONE',  ( 0.02062928380395624012, 0.1804553015353551615, -1.242749888402949976 ) ) ;
#20838 = DIRECTION ( 'NONE',  ( -1.000000000000000000, 0.000000000000000000, 1.224646799147353207E-16 ) ) ;
#20839 = CARTESIAN_POINT ( 'NONE',  ( -0.2764156081756484196, 1.692557448933383907E-17, 0.2063888888888917028 ) ) ;
#20840 = CARTESIAN_POINT ( 'NONE',  ( 2.064578755398029967E-15, 5.043833333485014947, -0.3119999999999999996 ) ) ;
#20841 = CARTESIAN_POINT ( 'NONE',  ( -0.1532564258214290931, 2.740000000000000213, -0.2654479161091319872 ) ) ;
#20842 = APPROVAL_PERSON_ORGANIZATION ( #3973, #15224, #18976 ) ;
#20843 = CARTESIAN_POINT ( 'NONE',  ( 0.3120000000000000551, 4.741749999999998799, 0.1292346314604056190 ) ) ;
#20844 = CARTESIAN_POINT ( 'NONE',  ( 0.2206173157302028232, 0.1916666666666663466, -0.2206173157302028232 ) ) ;
#20845 = CARTESIAN_POINT ( 'NONE',  ( 0.3119999999999999996, 5.130638888888888083, 0.1292346314604056190 ) ) ;
#20846 = CARTESIAN_POINT ( 'NONE',  ( 0.2819296736111110979, 4.224388888964755395, 0.1167790944451422425 ) ) ;
#20847 = CARTESIAN_POINT ( 'NONE',  ( -0.2977072594216396695, 1.822931211668208286E-17, 0.4093739260883065278 ) ) ;
#20848 = CARTESIAN_POINT ( 'NONE',  ( -0.1514837979169837701, 0.4428147562410876259, 0.4304954382810343150 ) ) ;
#20849 = DIRECTION ( 'NONE',  ( -0.000000000000000000, -1.000000000000000000, -0.000000000000000000 ) ) ;
#20850 = ORIENTED_EDGE ( 'NONE', *, *, #17960, .F. ) ;
#20851 = ORIENTED_EDGE ( 'NONE', *, *, #3016, .T. ) ;
#20852 = CARTESIAN_POINT ( 'NONE',  ( 0.4000000000000000222, 0.3196428569477723358, 0.000000000000000000 ) ) ;
#20853 = CARTESIAN_POINT ( 'NONE',  ( 0.2819296736111110979, 4.769527777853642903, -3.452642723725051716E-17 ) ) ;
#20854 = VECTOR ( 'NONE', #3117, 39.37007874015748143 ) ;
#20855 = LINE ( 'NONE', #2330, #20420 ) ;
#20856 = ADVANCED_FACE ( 'NONE', ( #10605 ), #9495, .F. ) ;
#20857 = DIRECTION ( 'NONE',  ( -2.498001805406602216E-16, -8.326672684688674053E-17, 1.000000000000000000 ) ) ;
#20858 = CARTESIAN_POINT ( 'NONE',  ( -0.3084988159814148201, 0.02958440236016895986, -0.09766548264808183610 ) ) ;
#20859 = CARTESIAN_POINT ( 'NONE',  ( 0.1993543840281267465, 4.220916666742532186, 0.1993543840281266633 ) ) ;
#20860 = APPROVAL_STATUS ( 'not_yet_approved' ) ;
#20861 = CARTESIAN_POINT ( 'NONE',  ( 7.459700445346810805E-07, 4.043833313442511290, -0.3119999999991081574 ) ) ;
#20862 = CARTESIAN_POINT ( 'NONE',  ( -0.1954553509668046918, -0.1954553509668046640, -0.008888888888887799475 ) ) ;
#20863 = CARTESIAN_POINT ( 'NONE',  ( 0.000000000000000000, 5.384999999999999787, -0.3119999999999999996 ) ) ;
#20864 = VERTEX_POINT ( 'NONE', #17047 ) ;
#20865 = CIRCLE ( 'NONE', #15428, 0.3150000000000000022 ) ;
#20866 = CARTESIAN_POINT ( 'NONE',  ( -0.1993543840281267465, 0.3618055554796889561, 0.1993543840281266633 ) ) ;
#20867 = CARTESIAN_POINT ( 'NONE',  ( -0.2663696356376525909, 5.203905143399228272, 0.09717633342841931754 ) ) ;
#20868 = CARTESIAN_POINT ( 'NONE',  ( 0.3999999999999999667, 0.2607142857142855652, -0.1299678784931625475 ) ) ;
#20869 = CARTESIAN_POINT ( 'NONE',  ( -0.3155070326520293400, 0.1306872919485614903, 0.1143750000000018641 ) ) ;
#20870 = CARTESIAN_POINT ( 'NONE',  ( 0.4687500000000002776, -0.04412582310964638377, 0.4181239759302315395 ) ) ;
#20871 = DIRECTION ( 'NONE',  ( -0.4999999999999913403, -0.000000000000000000, -0.8660254037844434816 ) ) ;
#20872 = CARTESIAN_POINT ( 'NONE',  ( -0.1167790944451424506, 0.5180555554796888451, 0.2819296736111110424 ) ) ;
#20873 = CARTESIAN_POINT ( 'NONE',  ( -0.2819296736111110979, 0.1777777777019111383, 0.1167790944451422425 ) ) ;
#20874 = EDGE_LOOP ( 'NONE', ( #9946, #8553, #1518, #13757 ) ) ;
#20875 = CARTESIAN_POINT ( 'NONE',  ( 0.2819296736111110424, 4.286888888964754507, -0.1167790944451423396 ) ) ;
#20876 = CARTESIAN_POINT ( 'NONE',  ( -0.3999999999999999667, 0.2089285712334865985, -0.1299678784931626030 ) ) ;
#20877 = CARTESIAN_POINT ( 'NONE',  ( 5.178964085587577574E-17, 4.880638888964754507, 0.2819296736111110979 ) ) ;
#20878 = CARTESIAN_POINT ( 'NONE',  ( 0.2819296736111110979, 4.273000000075865223, -0.1167790944451423396 ) ) ;
#20879 = CARTESIAN_POINT ( 'NONE',  ( 2.986000000000000210, 2.740000000000000213, -0.07500000000000014988 ) ) ;
#20880 = ORGANIZATION ( 'NAUO-ORG4', 'UNSPECIFIED', 'UNSPECIFIED' ) ;
#20881 = CARTESIAN_POINT ( 'NONE',  ( -0.1292346314604056745, 4.047305555707287894, -0.3119999999999999996 ) ) ;
#20882 = LINE ( 'NONE', #22832, #2125 ) ;
#20883 = AXIS2_PLACEMENT_3D ( 'NONE', #23995, #10607, #22174 ) ;
#20884 = VECTOR ( 'NONE', #4314, 39.37007874015748854 ) ;
#20885 = CARTESIAN_POINT ( 'NONE',  ( 0.1031051051775479510, -0.2870977370808670548, -0.09375409208931057004 ) ) ;
#20886 = ORIENTED_EDGE ( 'NONE', *, *, #2001, .T. ) ;
#20887 = B_SPLINE_CURVE_WITH_KNOTS ( 'NONE', 3,
 ( #19818, #16163, #23697, #5054, #8604, #17995, #10806, #14463, #21885, #18112, #1531, #12523, #16411, #23579, #3115, #21647, #23819, #17748, #19942, #7141, #14582, #1287, #1043, #22004, #21520, #4936, #5304, #5176, #6646, #3229, #12645, #17873, #20062, #12767, #2862, #10324, #8472, #15912 ),
 .UNSPECIFIED., .F., .F.,
 ( 4, 2, 2, 2, 2, 2, 2, 2, 2, 2, 2, 2, 2, 2, 2, 2, 2, 2, 4 ),
 ( 1.321750921635994236E-18, 0.001070994599891817887, 0.002141989199783634473, 0.003212983799675450409, 0.004283978399567268079, 0.005354972999459083581, 0.006425967599350898216, 0.007496962199242714585, 0.008567956799134529219, 0.009638951399026346456, 0.01070994599891816369, 0.01124544329886406971, 0.01178094059880997573, 0.01285193519870178776, 0.01392292979859359979, 0.01499392439848541356, 0.01606491899837722559, 0.01660041629832313334, 0.01713591359826903762 ),
 .UNSPECIFIED. ) ;
#20888 = DATE_TIME_ROLE ( 'creation_date' ) ;
#20889 = CARTESIAN_POINT ( 'NONE',  ( 0.2802773643484149924, 0.009513829220699975345, 0.3919440310150817952 ) ) ;
#20890 = CARTESIAN_POINT ( 'NONE',  ( -0.06305314479216488077, 0.03242967361111057795, 0.2752503750687063100 ) ) ;
#20891 = CARTESIAN_POINT ( 'NONE',  ( -0.5116234456863258950, 3.706421428007538488, -2.640781157734872320 ) ) ;
#20892 = ORIENTED_EDGE ( 'NONE', *, *, #19171, .T. ) ;
#20893 = CARTESIAN_POINT ( 'NONE',  ( -0.3119999999999999996, 0.5423611109593782231, 0.1292346314604056190 ) ) ;
#20894 = VERTEX_POINT ( 'NONE', #340 ) ;
#20895 = DIRECTION ( 'NONE',  ( -1.000000000000000000, -0.000000000000000000, -0.000000000000000000 ) ) ;
#20896 = CARTESIAN_POINT ( 'NONE',  ( -1.514244853754661224E-16, 0.5289902422706633800, 0.3941886329748526818 ) ) ;
#20897 = DIRECTION ( 'NONE',  ( 1.000000000000000000, 0.000000000000000000, 0.000000000000000000 ) ) ;
#20898 = CARTESIAN_POINT ( 'NONE',  ( 0.2233192592356399164, -0.01696428581182810730, 0.3073725909049500604 ) ) ;
#20899 = CARTESIAN_POINT ( 'NONE',  ( 0.3860879860166477329, 3.066692553488282957, 2.740461747820544414 ) ) ;
#20900 = ORIENTED_EDGE ( 'NONE', *, *, #23604, .F. ) ;
#20901 = EDGE_CURVE ( 'NONE', #18391, #10173, #17241, .T. ) ;
#20902 = CARTESIAN_POINT ( 'NONE',  ( -0.2923287055106771337, 0.2544642856167432798, -0.2123892367102620804 ) ) ;
#20903 = LINE ( 'NONE', #3960, #14667 ) ;
#20904 = EDGE_CURVE ( 'NONE', #6065, #21824, #2119, .T. ) ;
#20905 = CARTESIAN_POINT ( 'NONE',  ( -0.1993543840281266910, 4.068138888964754507, -0.1993543840281266910 ) ) ;
#20906 = LINE ( 'NONE', #22622, #4001 ) ;
#20907 = CARTESIAN_POINT ( 'NONE',  ( 0.1357040439698322387, 5.122023438247767402, 0.2773560592096749877 ) ) ;
#20908 = CARTESIAN_POINT ( 'NONE',  ( -0.2380092882192336723, 5.172599870306766157, -0.1756940437445040915 ) ) ;
#20909 = CARTESIAN_POINT ( 'NONE',  ( 0.3119999999999999996, 4.807722222373953969, -3.820898013339742174E-17 ) ) ;
#20910 = EDGE_CURVE ( 'NONE', #20999, #3235, #5251, .T. ) ;
#20911 = CARTESIAN_POINT ( 'NONE',  ( -0.2819296736111110424, 4.981333333409200037, 0.1167790944451424923 ) ) ;
#20912 = ORIENTED_EDGE ( 'NONE', *, *, #16802, .F. ) ;
#20913 = CARTESIAN_POINT ( 'NONE',  ( 0.2819296736111110979, 4.213972222298087544, -3.452642723725051716E-17 ) ) ;
#20914 = ORIENTED_EDGE ( 'NONE', *, *, #4199, .F. ) ;
#20915 = CARTESIAN_POINT ( 'NONE',  ( 0.2923287055106771337, 0.1437499999024575981, -0.2123892367102620249 ) ) ;
#20916 = ORIENTED_EDGE ( 'NONE', *, *, #6180, .F. ) ;
#20917 = VERTEX_POINT ( 'NONE', #23994 ) ;
#20918 = DATE_AND_TIME ( #9708, #18512 ) ;
#20919 = ORIENTED_EDGE ( 'NONE', *, *, #12330, .F. ) ;
#20920 = CARTESIAN_POINT ( 'NONE',  ( 0.3155070326520292845, -5.795770164686806123E-17, 0.4268750000000047784 ) ) ;
#20921 = CARTESIAN_POINT ( 'NONE',  ( 0.1292346314604057300, 0.2854166666666662633, 0.3119999999999998885 ) ) ;
#20922 = CARTESIAN_POINT ( 'NONE',  ( 0.1993543840281267465, 3.832027777853643791, 0.1993543840281266633 ) ) ;
#20923 = DIRECTION ( 'NONE',  ( -0.000000000000000000, -1.000000000000000000, -0.000000000000000000 ) ) ;
#20924 = CARTESIAN_POINT ( 'NONE',  ( 0.2206173157302028787, 4.627166666666665762, 0.2206173157302027954 ) ) ;
#20925 = ADVANCED_FACE ( 'NONE', ( #22411 ), #22171, .T. ) ;
#20926 = CARTESIAN_POINT ( 'NONE',  ( 0.3146277125502771610, -0.3722332453489731741, 0.07156651416103082530 ) ) ;
#20927 = EDGE_CURVE ( 'NONE', #22119, #9702, #1806, .T. ) ;
#20928 = CARTESIAN_POINT ( 'NONE',  ( 0.1144950937579611444, 0.2764156081756483641, 0.2931944444444479769 ) ) ;
#20929 = CARTESIAN_POINT ( 'NONE',  ( -5.178964085587577574E-17, 0.4243055554796889006, 0.2819296736111110979 ) ) ;
#20930 = CARTESIAN_POINT ( 'NONE',  ( -0.1144950937579609918, -0.2764156081756484196, 0.3834722222222265442 ) ) ;
#20931 = ORIENTED_EDGE ( 'NONE', *, *, #19928, .T. ) ;
#20932 = EDGE_CURVE ( 'NONE', #5628, #17172, #17319, .T. ) ;
#20933 = CARTESIAN_POINT ( 'NONE',  ( 5.178964085587577574E-17, 4.713972222298088433, 0.2819296736111110979 ) ) ;
#20934 = CARTESIAN_POINT ( 'NONE',  ( 0.2956865686883918820, 4.471526487522247351, 0.1000891740342018943 ) ) ;
#20935 = CARTESIAN_POINT ( 'NONE',  ( -0.1993543840281266355, 4.693138888964754507, 0.1993543840281267465 ) ) ;
#20936 = DIRECTION ( 'NONE',  ( -0.000000000000000000, -1.000000000000000000, -0.000000000000000000 ) ) ;
#20937 = CARTESIAN_POINT ( 'NONE',  ( 0.2218613123050385549, 4.870266018951173947, -0.2206117788904509158 ) ) ;
#20938 = CARTESIAN_POINT ( 'NONE',  ( -0.1963981168484050244, -1.109535145422192752E-16, 0.3299405160370264545 ) ) ;
#20939 = CARTESIAN_POINT ( 'NONE',  ( 0.000000000000000000, 0.1199999999999999956, -0.2109499999999996656 ) ) ;
#20940 = CARTESIAN_POINT ( 'NONE',  ( 5.731347020009612645E-17, 4.342444444444443441, 0.3119999999999999996 ) ) ;
#20941 = AXIS2_PLACEMENT_3D ( 'NONE', #9455, #22736, #1895 ) ;
#20942 = CARTESIAN_POINT ( 'NONE',  ( 0.2819296736111111534, 3.766055555631421026, 0.1167790944451422563 ) ) ;
#20943 = EDGE_CURVE ( 'NONE', #3460, #9832, #6245, .T. ) ;
#20944 = FACE_OUTER_BOUND ( 'NONE', #7156, .T. ) ;
#20945 = ORIENTED_EDGE ( 'NONE', *, *, #6757, .F. ) ;
#20946 = CARTESIAN_POINT ( 'NONE',  ( 0.3115085581940752468, 4.585014881649954965, 0.01788609438656960440 ) ) ;
#20947 = VERTEX_POINT ( 'NONE', #11692 ) ;
#20948 = CARTESIAN_POINT ( 'NONE',  ( 0.06090392925245493444, 4.708829327785332808, -0.3064243836155239320 ) ) ;
#20949 = CARTESIAN_POINT ( 'NONE',  ( 0.2764156081756484196, -5.077672346800151106E-17, 0.4494444444444492537 ) ) ;
#20950 = AXIS2_PLACEMENT_3D ( 'NONE', #22750, #15442, #11913 ) ;
#20951 = CARTESIAN_POINT ( 'NONE',  ( 0.3120466542833977841, 4.308815547343077590, -0.04051276955858209433 ) ) ;
#20952 = ORIENTED_EDGE ( 'NONE', *, *, #10068, .F. ) ;
#20953 = EDGE_CURVE ( 'NONE', #5711, #5262, #18487, .T. ) ;
#20954 = CARTESIAN_POINT ( 'NONE',  ( -0.2923287055106771337, 0.4116071427596003640, 0.2123892367102619971 ) ) ;
#20955 = EDGE_CURVE ( 'NONE', #606, #20467, #7350, .T. ) ;
#20956 = CARTESIAN_POINT ( 'NONE',  ( -0.1167790944451422702, 0.4972222221463556413, -0.2819296736111110424 ) ) ;
#20957 = CARTESIAN_POINT ( 'NONE',  ( -0.009764748067830458442, 5.206640035683669510, 0.2819296736110837309 ) ) ;
#20958 = CARTESIAN_POINT ( 'NONE',  ( 0.2501637473317315230, 0.6631371529007064058, -1.085132529289236425 ) ) ;
#20959 = CARTESIAN_POINT ( 'NONE',  ( 0.1292346314604056745, 0.5284722222222218990, -0.3119999999999999996 ) ) ;
#20960 = CARTESIAN_POINT ( 'NONE',  ( -0.2764156081756484196, 0.1144950937579609918, 0.1473611111111134686 ) ) ;
#20961 = CARTESIAN_POINT ( 'NONE',  ( -0.09977969951898062184, 5.115641765141615949, 0.2926989633898121057 ) ) ;
#20962 = CARTESIAN_POINT ( 'NONE',  ( -0.01277271335453335384, 0.5470360373338563065, 0.04287645741408798589 ) ) ;
#20963 = CARTESIAN_POINT ( 'NONE',  ( -0.3125000000000000000, 1.913510623667739771E-17, 0.3452777777777818469 ) ) ;
#20964 = CARTESIAN_POINT ( 'NONE',  ( -5.731347020009612645E-17, 0.2263888888888885564, 0.3119999999999999996 ) ) ;
#20965 = CARTESIAN_POINT ( 'NONE',  ( 0.2206173157302027954, 5.085499999999998799, -0.2206173157302028232 ) ) ;
#20966 = CARTESIAN_POINT ( 'NONE',  ( -0.2819296736111110424, 4.141055555631421470, -0.1167790944451423119 ) ) ;
#20967 = CARTESIAN_POINT ( 'NONE',  ( -1.910449006669871087E-17, 3.814666666666665762, -0.3119999999999999996 ) ) ;
#20968 = CARTESIAN_POINT ( 'NONE',  ( 0.2472135954999579166, 0.3803571426620580564, 0.3402603233408160732 ) ) ;
#20969 = ORIENTED_EDGE ( 'NONE', *, *, #15576, .T. ) ;
#20970 = EDGE_LOOP ( 'NONE', ( #13645, #10549, #20773, #20886 ) ) ;
#20971 = CARTESIAN_POINT ( 'NONE',  ( -0.1167790944451423535, 4.807722222298087544, 0.2819296736111110424 ) ) ;
#20972 = CARTESIAN_POINT ( 'NONE',  ( -0.3613381517857143232, 0.3151785713310290005, -4.425116109941954795E-17 ) ) ;
#20973 = CARTESIAN_POINT ( 'NONE',  ( 0.000000000000000000, 3.700000000000000622, -0.4000000000000000222 ) ) ;
#20974 =( NAMED_UNIT ( * ) PLANE_ANGLE_UNIT ( ) SI_UNIT ( $, .RADIAN. ) );
#20975 = CARTESIAN_POINT ( 'NONE',  ( 0.02244429927890741541, 3.709892914452737500, -0.3112240927256947898 ) ) ;
#20976 = CARTESIAN_POINT ( 'NONE',  ( -1.726321361862525858E-17, 4.297305555631421470, -0.2819296736111110979 ) ) ;
#20977 = APPROVAL_STATUS ( 'not_yet_approved' ) ;
#20978 = CARTESIAN_POINT ( 'NONE',  ( -0.01914896636169877847, 4.044354364280504655, -0.3114118915433974344 ) ) ;
#20979 = CARTESIAN_POINT ( 'NONE',  ( -0.1144950937579609918, -0.2764156081756484196, -0.06097222222222156013 ) ) ;
#20980 = CARTESIAN_POINT ( 'NONE',  ( -0.3125000000000000000, 1.913510623667739771E-17, 0.1230555555555578606 ) ) ;
#20981 = VECTOR ( 'NONE', #22164, 39.37007874015748143 ) ;
#20982 = CARTESIAN_POINT ( 'NONE',  ( -0.2819296736111110424, 0.3513888888130222155, -0.1167790944451423396 ) ) ;
#20983 = FACE_OUTER_BOUND ( 'NONE', #1133, .T. ) ;
#20984 = CARTESIAN_POINT ( 'NONE',  ( 0.1294417382415921358, -0.3125000000000002220, 0.1890277777777802926 ) ) ;
#20985 = CARTESIAN_POINT ( 'NONE',  ( 0.1236067977499789861, 0.3428571428571428048, -0.3804226065180614236 ) ) ;
#20986 = CARTESIAN_POINT ( 'NONE',  ( 0.000000000000000000, 0.3155070326520292845, 0.1039583333333351234 ) ) ;
#20987 = LINE ( 'NONE', #9786, #5600 ) ;
#20988 = CARTESIAN_POINT ( 'NONE',  ( 0.2206173157302027954, 5.029944444444443441, -0.2206173157302028232 ) ) ;
#20989 = CARTESIAN_POINT ( 'NONE',  ( 0.1993543840281266910, 0.5423611110352445364, -0.1993543840281266910 ) ) ;
#20990 = CARTESIAN_POINT ( 'NONE',  ( 0.1167790944451423535, 0.1361111110352444808, 0.2819296736111110424 ) ) ;
#20991 = VERTEX_POINT ( 'NONE', #14478 ) ;
#20992 = CARTESIAN_POINT ( 'NONE',  ( 0.2819296736111110979, 4.227861111186976828, -3.452642723725051716E-17 ) ) ;
#20993 = CARTESIAN_POINT ( 'NONE',  ( -7.726019084026502927E-17, 0.2303571426620580065, 0.4205848896953069405 ) ) ;
#20994 = ADVANCED_FACE ( 'NONE', ( #19960 ), #3131, .F. ) ;
#20995 = CARTESIAN_POINT ( 'NONE',  ( -1.726321361862525858E-17, 4.908416666742532186, -0.2819296736111110979 ) ) ;
#20996 = EDGE_CURVE ( 'NONE', #20917, #20185, #18103, .T. ) ;
#20997 = CARTESIAN_POINT ( 'NONE',  ( 5.178964085587577574E-17, 4.255638888964754507, 0.2819296736111110979 ) ) ;
#20998 = CYLINDRICAL_SURFACE ( 'NONE', #11411, 0.3119999999999999996 ) ;
#20999 = VERTEX_POINT ( 'NONE', #23597 ) ;
#21000 = CARTESIAN_POINT ( 'NONE',  ( 0.2206173157302028787, 4.516055555555555046, 0.2206173157302027954 ) ) ;
#21001 = CARTESIAN_POINT ( 'NONE',  ( 0.3119999999999999996, 3.807722222373953969, -3.820898013339742174E-17 ) ) ;
#21002 = CARTESIAN_POINT ( 'NONE',  ( -0.2530612899223193546, 0.3951608735071495127, 0.4181572966874577135 ) ) ;
#21003 = VECTOR ( 'NONE', #729, 39.37007874015748143 ) ;
#21004 = CARTESIAN_POINT ( 'NONE',  ( -0.04581704741057199964, -0.3043534538584903304, -0.09649300259420087733 ) ) ;
#21005 = ORIENTED_EDGE ( 'NONE', *, *, #20468, .F. ) ;
#21006 = PERSON_AND_ORGANIZATION ( #15518, #2538 ) ;
#21007 = CARTESIAN_POINT ( 'NONE',  ( 0.2472135954999579166, 0.4517857140906293423, 0.3402603233408160732 ) ) ;
#21008 = CARTESIAN_POINT ( 'NONE',  ( -0.2368311528898977558, 5.008462562740330526, 0.2031552041900300254 ) ) ;
#21009 = EDGE_LOOP ( 'NONE', ( #8861, #12237, #1119, #14444, #22167 ) ) ;
#21010 = CARTESIAN_POINT ( 'NONE',  ( 0.3119999999999998885, 0.6187499998482670627, 0.1292346314604058410 ) ) ;
#21011 = ORIENTED_EDGE ( 'NONE', *, *, #12041, .F. ) ;
#21012 = CARTESIAN_POINT ( 'NONE',  ( 0.1915112473476633104, 4.244112575941767496, 0.2496615136355418429 ) ) ;
#21013 = CARTESIAN_POINT ( 'NONE',  ( 0.3874422277197113185, 0.3175760028958486414, 0.4114235598616964862 ) ) ;
#21014 = CARTESIAN_POINT ( 'NONE',  ( 0.000000000000000000, 3.738758431839877614E-19, -0.1016666666666665164 ) ) ;
#21015 = CARTESIAN_POINT ( 'NONE',  ( -6.979263641208234666E-17, -0.02410714295468524906, 0.3799334167787516425 ) ) ;
#21016 = CARTESIAN_POINT ( 'NONE',  ( 0.2640909437941768578, 5.182232675516351250, -0.1266275688248941766 ) ) ;
#21017 =( BOUNDED_CURVE ( )  B_SPLINE_CURVE ( 2, ( #9552, #22710, #2361, #15405, #9309, #4176, #13466, #7717, #400 ),
 .UNSPECIFIED., .F., .T. ) 
 B_SPLINE_CURVE_WITH_KNOTS ( ( 3, 2, 2, 2, 3 ),
 ( 0.2291666666666666574, 0.2395833333333333426, 0.2500000000000000000, 0.2604166666666666852, 0.2708333333333333148 ),
 .UNSPECIFIED. ) 
 CURVE ( )  GEOMETRIC_REPRESENTATION_ITEM ( )  RATIONAL_B_SPLINE_CURVE ( ( 1.000000000000000000, 0.9238795325112867385, 1.000000000000000000, 0.9238795325112867385, 1.000000000000000000, 0.9238795325112867385, 1.000000000000000000, 0.9238795325112867385, 1.000000000000000000 ) ) 
 REPRESENTATION_ITEM ( '' )  );
#21018 = CC_DESIGN_DATE_AND_TIME_ASSIGNMENT ( #7987, #22634, ( #5255 ) ) ;
#21019 = ORIENTED_EDGE ( 'NONE', *, *, #14994, .T. ) ;
#21020 = CARTESIAN_POINT ( 'NONE',  ( 0.2923287055106771337, 0.3758928570453146656, -0.2123892367102620249 ) ) ;
#21021 = VECTOR ( 'NONE', #3954, 39.37007874015748143 ) ;
#21022 = DIRECTION ( 'NONE',  ( -0.5000000000000037748, 0.000000000000000000, -0.8660254037844362651 ) ) ;
#21023 = CARTESIAN_POINT ( 'NONE',  ( 0.2764156081756483641, -0.1144950937579611167, 0.4459722222222269328 ) ) ;
#21024 = CARTESIAN_POINT ( 'NONE',  ( -0.1993543840281266910, 3.957027777853642903, -0.1993543840281266910 ) ) ;
#21025 = DIRECTION ( 'NONE',  ( -0.000000000000000000, -0.9961946980917454342, 0.08715574274765830465 ) ) ;
#21026 = CARTESIAN_POINT ( 'NONE',  ( -0.2928190810534017641, 5.180208114765485483, 0.01414289444493066483 ) ) ;
#21027 = CARTESIAN_POINT ( 'NONE',  ( 0.1292346314604058410, 4.630638889040620931, 0.3119999999999998885 ) ) ;
#21028 = CARTESIAN_POINT ( 'NONE',  ( -0.1993543840281266355, 5.040361111186977716, 0.1993543840281267465 ) ) ;
#21029 = ORIENTED_EDGE ( 'NONE', *, *, #9294, .T. ) ;
#21030 = CARTESIAN_POINT ( 'NONE',  ( -0.2819296736111110424, 4.349388888964754507, -0.1167790944451423119 ) ) ;
#21031 = EDGE_LOOP ( 'NONE', ( #14832, #7629, #5243, #17661 ) ) ;
#21032 = CARTESIAN_POINT ( 'NONE',  ( -0.2233192592356399442, 0.3044642856167432132, -0.3073725909049499494 ) ) ;
#21033 = ORIENTED_EDGE ( 'NONE', *, *, #11314, .T. ) ;
#21034 = VECTOR ( 'NONE', #14159, 39.37007874015748854 ) ;
#21035 = EDGE_CURVE ( 'NONE', #789, #23019, #12592, .T. ) ;
#21036 = VECTOR ( 'NONE', #2937, 39.37007874015748854 ) ;
#21037 = VERTEX_POINT ( 'NONE', #4713 ) ;
#21038 = EDGE_CURVE ( 'NONE', #2739, #20728, #15218, .T. ) ;
#21039 = DATE_AND_TIME ( #7868, #4091 ) ;
#21040 = CARTESIAN_POINT ( 'NONE',  ( 0.3116633505738114485, 3.673292957400295933, -0.09499999999999995948 ) ) ;
#21041 = CARTESIAN_POINT ( 'NONE',  ( 0.000000000000000000, 5.384999999999999787, 0.000000000000000000 ) ) ;
#21042 = CARTESIAN_POINT ( 'NONE',  ( -0.1292346314604056190, 0.1395833331816004053, -0.3119999999999999996 ) ) ;
#21043 = CARTESIAN_POINT ( 'NONE',  ( 0.08947733366648276399, 4.407491422679668425, 0.2989658942065363534 ) ) ;
#21045 = EDGE_CURVE ( 'NONE', #13469, #17766, #19447, .T. ) ;
#21044 = LINE ( 'NONE', #15446, #23685 ) ;
#21046 = CARTESIAN_POINT ( 'NONE',  ( -1.910449006669871087E-17, 4.925777777777777366, -0.3119999999999999996 ) ) ;
#21047 = CARTESIAN_POINT ( 'NONE',  ( -3.385114897866767815E-17, -0.2764156081756484196, 0.2133333333333362336 ) ) ;
#21048 = CARTESIAN_POINT ( 'NONE',  ( 1.726321361862525858E-17, 0.5631944443685776847, -0.2819296736111110979 ) ) ;
#21049 = CARTESIAN_POINT ( 'NONE',  ( 0.2764156081756484196, -5.077672346800151106E-17, -0.1061111111111107813 ) ) ;
#21050 = ORIENTED_EDGE ( 'NONE', *, *, #12539, .F. ) ;
#21051 = CARTESIAN_POINT ( 'NONE',  ( 0.2819296736111110424, 4.731333333409200925, -0.1167790944451423396 ) ) ;
#21052 = CARTESIAN_POINT ( 'NONE',  ( 0.01298396664829300738, -0.5473896884649182004, 0.04271845132552136437 ) ) ;
#21053 = CARTESIAN_POINT ( 'NONE',  ( 0.1993543840281267465, 4.707027777853643791, 0.1993543840281266633 ) ) ;
#21054 = CARTESIAN_POINT ( 'NONE',  ( -5.731347020009612645E-17, 0.2749999998482670627, 0.3119999999999999996 ) ) ;
#21055 = AXIS2_PLACEMENT_3D ( 'NONE', #23315, #10427, #12381 ) ;
#21056 = CARTESIAN_POINT ( 'NONE',  ( 0.2853224037306363869, 4.866967269276749164, -0.1262817630124163093 ) ) ;
#21057 = CARTESIAN_POINT ( 'NONE',  ( 3.820898013339742174E-17, 5.384999999999999787, 0.3119999999999999996 ) ) ;
#21058 = DIRECTION ( 'NONE',  ( 0.000000000000000000, 1.000000000000000000, 0.000000000000000000 ) ) ;
#21059 = CARTESIAN_POINT ( 'NONE',  ( 0.1292346314604058410, 4.179249999999998799, 0.3119999999999998885 ) ) ;
#21060 = CIRCLE ( 'NONE', #10554, 0.2500000000000000000 ) ;
#21061 = CARTESIAN_POINT ( 'NONE',  ( 0.1015006192750689679, 3.724843167714382286, -0.2819296736111111534 ) ) ;
#21062 = CARTESIAN_POINT ( 'NONE',  ( -1.054647954922321762E-07, 4.988277780858759947, -0.3119999999999820695 ) ) ;
#21063 = ORIENTED_EDGE ( 'NONE', *, *, #22252, .F. ) ;
#21064 = CARTESIAN_POINT ( 'NONE',  ( 0.3125000000000000555, -5.740531871003217465E-17, 0.1994444444444470055 ) ) ;
#21065 = ORIENTED_EDGE ( 'NONE', *, *, #14087, .F. ) ;
#21066 = CARTESIAN_POINT ( 'NONE',  ( 0.1554048093938449615, 4.687324857274296264, 0.2736299092323108972 ) ) ;
#21067 = CARTESIAN_POINT ( 'NONE',  ( 0.4641461581055187358, -0.2728099291808114280, 0.04698409998688660855 ) ) ;
#21068 = CARTESIAN_POINT ( 'NONE',  ( 0.2764156081756483641, 0.1144950937579610056, 0.3973611111111154393 ) ) ;
#21069 = CIRCLE ( 'NONE', #13699, 0.3119999999999999996 ) ;
#21070 = CARTESIAN_POINT ( 'NONE',  ( 0.04078035003190004504, 4.294990863552893501, 0.3120001095418362125 ) ) ;
#21071 = EDGE_CURVE ( 'NONE', #1241, #20894, #20822, .T. ) ;
#21072 = ORIENTED_EDGE ( 'NONE', *, *, #18104, .T. ) ;
#21073 = CARTESIAN_POINT ( 'NONE',  ( 0.2233192592356399164, 0.4294642856167432687, 0.3073725909049500604 ) ) ;
#21074 = CARTESIAN_POINT ( 'NONE',  ( 1.726321361862525858E-17, 0.5493055554796888451, -0.2819296736111110979 ) ) ;
#21075 = CARTESIAN_POINT ( 'NONE',  ( -0.1317548836793264455, 5.206640035683668621, 0.2500202773221226193 ) ) ;
#21076 = CARTESIAN_POINT ( 'NONE',  ( 0.2505061212867025211, 0.2922223361170756539, -1.186846436122991788 ) ) ;
#21077 = CARTESIAN_POINT ( 'NONE',  ( -0.1689451345729832410, -0.2321341939677299682, -0.07613786318562981714 ) ) ;
#21078 = CARTESIAN_POINT ( 'NONE',  ( 0.2764156081756484196, -5.077672346800151106E-17, 0.1786111111111136907 ) ) ;
#21079 = VERTEX_POINT ( 'NONE', #7513 ) ;
#21080 = PLANE ( 'NONE',  #9507 ) ;
#21081 = CARTESIAN_POINT ( 'NONE',  ( 0.3999999999999999667, 0.1017857140906294616, 0.1299678784931626307 ) ) ;
#21082 = CARTESIAN_POINT ( 'NONE',  ( 0.3084175934503982641, -2.427762526784286478E-18, -0.1882653658700420007 ) ) ;
#21083 = CARTESIAN_POINT ( 'NONE',  ( -5.731347020009612645E-17, 0.2819444444444441089, 0.3119999999999999996 ) ) ;
#21084 = CARTESIAN_POINT ( 'NONE',  ( -0.1292346314604056745, 4.873694444444444329, -0.3119999999999999996 ) ) ;
#21085 = CARTESIAN_POINT ( 'NONE',  ( -0.2819296736111110424, 3.981333333409199593, 0.1167790944451424923 ) ) ;
#21086 = CARTESIAN_POINT ( 'NONE',  ( -0.04085484144393203287, 4.322780934022267374, -0.3119999999289135850 ) ) ;
#21087 = DIRECTION ( 'NONE',  ( 0.000000000000000000, 0.000000000000000000, 1.000000000000000000 ) ) ;
#21088 = CARTESIAN_POINT ( 'NONE',  ( 0.3013753051098548297, 4.810095209863023413, -0.08402212184464949440 ) ) ;
#21089 = ORIENTED_EDGE ( 'NONE', *, *, #2142, .T. ) ;
#21090 = VERTEX_POINT ( 'NONE', #18611 ) ;
#21091 = CARTESIAN_POINT ( 'NONE',  ( 0.3084988159814222586, 0.02958440236011267849, 0.4201654826480894500 ) ) ;
#21092 = CARTESIAN_POINT ( 'NONE',  ( 0.2819296736111110979, 4.710500000075865223, 0.1167790944451422425 ) ) ;
#21093 = CARTESIAN_POINT ( 'NONE',  ( 0.01848103877824613592, -0.5441716683897390716, 0.04413116910601658227 ) ) ;
#21094 = EDGE_CURVE ( 'NONE', #12631, #6271, #7591, .T. ) ;
#21095 = CARTESIAN_POINT ( 'NONE',  ( -0.09708543963280202860, 5.164879205389378392, 0.2826001691826344753 ) ) ;
#21096 = EDGE_CURVE ( 'NONE', #3466, #12593, #3276, .T. ) ;
#21097 = EDGE_CURVE ( 'NONE', #17146, #20507, #13146, .T. ) ;
#21098 = MECHANICAL_CONTEXT ( 'NONE', #9823, 'mechanical' ) ;
#21099 = CARTESIAN_POINT ( 'NONE',  ( 3.827021247335479543E-17, 0.4997679491924311157, 0.3125000000000001665 ) ) ;
#21100 = CARTESIAN_POINT ( 'NONE',  ( 0.000000000000000000, 5.384999999999999787, 0.000000000000000000 ) ) ;
#21101 = CARTESIAN_POINT ( 'NONE',  ( -0.2819296736111110979, 4.307722222298088433, -0.1167790944451422980 ) ) ;
#21102 = EDGE_CURVE ( 'NONE', #14570, #3466, #8497, .T. ) ;
#21103 = CARTESIAN_POINT ( 'NONE',  ( 0.3950000000000000178, 0.05000000000000028727, -1.966000000000000192 ) ) ;
#21104 = CARTESIAN_POINT ( 'NONE',  ( 0.1954553509668047195, 0.1954553509668046085, -0.03666666666666580643 ) ) ;
#21105 = DIRECTION ( 'NONE',  ( 0.5000000000000012212, 0.8660254037844380415, 0.000000000000000000 ) ) ;
#21106 = ORIENTED_EDGE ( 'NONE', *, *, #5635, .T. ) ;
#21107 = CARTESIAN_POINT ( 'NONE',  ( 0.2819296736111110424, 0.3791666665908000611, 0.1167790944451424923 ) ) ;
#21108 = CARTESIAN_POINT ( 'NONE',  ( 0.000000000000000000, 5.384999999999999787, 0.000000000000000000 ) ) ;
#21109 = CARTESIAN_POINT ( 'NONE',  ( -1.910449006669871087E-17, 4.481333333333331836, -0.3119999999999999996 ) ) ;
#21110 = CARTESIAN_POINT ( 'NONE',  ( -0.4000000000000000222, 0.3678571428571427715, 0.1299678784931624920 ) ) ;
#21111 = CARTESIAN_POINT ( 'NONE',  ( 0.3155070326520292845, -5.795770164686806123E-17, 0.2011805555555581104 ) ) ;
#21112 = DIRECTION ( 'NONE',  ( -0.000000000000000000, -1.000000000000000000, -0.000000000000000000 ) ) ;
#21113 = CARTESIAN_POINT ( 'NONE',  ( -0.4805070082343984583, -0.2560807851245831546, 0.04413116910601652676 ) ) ;
#21114 = CARTESIAN_POINT ( 'NONE',  ( 0.1167790944451423119, 0.3791666665908000611, -0.2819296736111110979 ) ) ;
#21115 = CARTESIAN_POINT ( 'NONE',  ( 1.726321361862525858E-17, 0.1604166665908000333, -0.2819296736111110979 ) ) ;
#21116 = VERTEX_POINT ( 'NONE', #23922 ) ;
#21117 = CARTESIAN_POINT ( 'NONE',  ( -1.726321361862525858E-17, 3.963972222298087988, -0.2819296736111110979 ) ) ;
#21118 = CARTESIAN_POINT ( 'NONE',  ( 0.3999999999999999667, 0.3160714283763437216, 0.1299678784931626307 ) ) ;
#21119 = CARTESIAN_POINT ( 'NONE',  ( 0.2819296736111110424, 4.786888888964755395, -0.1167790944451423396 ) ) ;
#21120 =( BOUNDED_CURVE ( )  B_SPLINE_CURVE ( 2, ( #21952, #10872, #14779, #120, #18658, #20609, #9152, #22312, #9035 ),
 .UNSPECIFIED., .F., .F. ) 
 B_SPLINE_CURVE_WITH_KNOTS ( ( 3, 2, 2, 2, 3 ),
 ( 0.1458333333333333426, 0.1562500000000000000, 0.1666666666666666574, 0.1770833333333333426, 0.1875000000000000000 ),
 .UNSPECIFIED. ) 
 CURVE ( )  GEOMETRIC_REPRESENTATION_ITEM ( )  RATIONAL_B_SPLINE_CURVE ( ( 1.000000000000000000, 0.9238795325112867385, 1.000000000000000000, 0.9238795325112867385, 1.000000000000000000, 0.9238795325112867385, 1.000000000000000000, 0.9238795325112867385, 1.000000000000000000 ) ) 
 REPRESENTATION_ITEM ( '' )  );
#21121 = CARTESIAN_POINT ( 'NONE',  ( 0.3122281832482405317, 5.078663991669950306, -0.005250876328984169575 ) ) ;
#21122 = ORIENTED_EDGE ( 'NONE', *, *, #19683, .F. ) ;
#21123 = DIRECTION ( 'NONE',  ( -0.8660254037844382635, 6.853229114107538658E-30, 0.5000000000000004441 ) ) ;
#21124 = CARTESIAN_POINT ( 'NONE',  ( 5.731347020009612645E-17, 3.793833333485065573, 0.3119999999999999996 ) ) ;
#21125 = DIRECTION ( 'NONE',  ( -0.000000000000000000, -1.000000000000000000, -0.000000000000000000 ) ) ;
#21126 = ORIENTED_EDGE ( 'NONE', *, *, #17863, .F. ) ;
#21127 = EDGE_CURVE ( 'NONE', #10864, #2273, #23799, .T. ) ;
#21128 = APPROVAL_DATE_TIME ( #10288, #22227 ) ;
#21129 = CIRCLE ( 'NONE', #2041, 0.2510000000000000009 ) ;
#21130 = EDGE_CURVE ( 'NONE', #20864, #23410, #4445, .T. ) ;
#21131 = CARTESIAN_POINT ( 'NONE',  ( 0.06335377612981404893, 0.3445980613733267695, -0.4000000000000001887 ) ) ;
#21132 = CARTESIAN_POINT ( 'NONE',  ( -0.3516234456863258084, 4.901168349308694161, -2.733157200805212295 ) ) ;
#21133 = EDGE_LOOP ( 'NONE', ( #3244, #21182, #14294, #15901, #12128 ) ) ;
#21134 = CARTESIAN_POINT ( 'NONE',  ( 0.2819296736111110979, 0.04930555547968892144, 0.000000000000000000 ) ) ;
#21135 = ORIENTED_EDGE ( 'NONE', *, *, #11289, .T. ) ;
#21136 = CARTESIAN_POINT ( 'NONE',  ( 0.2659125765915840711, 4.257081166359744984, -0.1637272094895568519 ) ) ;
#21137 = CARTESIAN_POINT ( 'NONE',  ( 0.000000000000000000, 5.384999999999999787, 0.000000000000000000 ) ) ;
#21138 = CARTESIAN_POINT ( 'NONE',  ( 0.2552298690385793600, 4.090937613976504572, -0.1843366434591496850 ) ) ;
#21139 = CARTESIAN_POINT ( 'NONE',  ( -0.3613381517857143232, 0.3116071427596003862, -0.1174058825155741004 ) ) ;
#21140 = PLANE ( 'NONE',  #20207 ) ;
#21141 = B_SPLINE_CURVE_WITH_KNOTS ( 'NONE', 3,
 ( #16190, #5073, #23239, #10111, #17534, #827, #8257, #15706, #23121, #13885 ),
 .UNSPECIFIED., .F., .F.,
 ( 4, 2, 2, 2, 4 ),
 ( 0.000000000000000000, 0.003321633220911225995, 0.006643266441822451990, 0.009964899662733674515, 0.01328653288364490051 ),
 .UNSPECIFIED. ) ;
#21142 = VERTEX_POINT ( 'NONE', #16508 ) ;
#21143 = CARTESIAN_POINT ( 'NONE',  ( 0.2923287055106771337, 0.3616071427596004306, 0.2123892367102621359 ) ) ;
#21144 = CARTESIAN_POINT ( 'NONE',  ( 2.319244702705236083, 2.291712385858714729, -2.476240473580833434 ) ) ;
#21145 = CARTESIAN_POINT ( 'NONE',  ( 0.1993543840281267465, 4.095916666742532186, 0.1993543840281266633 ) ) ;
#21146 = B_SPLINE_CURVE_WITH_KNOTS ( 'NONE', 3,
 ( #8640, #962, #15728, #12088, #8277, #4504, #19739, #1087, #17434, #8156, #3038, #8519, #23142, #14022, #21213, #15610, #2912, #19857 ),
 .UNSPECIFIED., .F., .F.,
 ( 4, 2, 2, 2, 2, 2, 2, 2, 4 ),
 ( 0.7949730820619140825, 0.7972563070159356391, 0.7995395319699570846, 0.8018227569239786412, 0.8041059818780001978, 0.8063892068320216433, 0.8086724317860431999, 0.8109556567400646454, 0.8132388816940862020 ),
 .UNSPECIFIED. ) ;
#21147 = CARTESIAN_POINT ( 'NONE',  ( -0.09380593400082881672, 0.03242967361111052244, 0.2658661084243340578 ) ) ;
#21148 = CARTESIAN_POINT ( 'NONE',  ( -0.2548359695741092557, 5.185457950352025946, 0.1418493590379871494 ) ) ;
#21149 = CARTESIAN_POINT ( 'NONE',  ( 0.2206173157302027954, 4.592444444596176290, -0.2206173157302028232 ) ) ;
#21150 = AXIS2_PLACEMENT_3D ( 'NONE', #17136, #11532, #13725 ) ;
#21151 = CARTESIAN_POINT ( 'NONE',  ( 0.2819296736111110979, 4.838972222298088433, -3.452642723725051716E-17 ) ) ;
#21152 = ORIENTED_EDGE ( 'NONE', *, *, #21842, .T. ) ;
#21153 = CARTESIAN_POINT ( 'NONE',  ( -0.1167790944451423535, 3.974388888964754063, 0.2819296736111110424 ) ) ;
#21154 = ORIENTED_EDGE ( 'NONE', *, *, #22834, .T. ) ;
#21155 = EDGE_LOOP ( 'NONE', ( #6679, #1494, #8275, #17129 ) ) ;
#21156 = APPROVAL_STATUS ( 'not_yet_approved' ) ;
#21157 = EDGE_LOOP ( 'NONE', ( #16570, #23480, #16117, #4413, #18173, #16180, #5381, #23419, #24057, #17013, #2792, #13351, #1479, #17410, #17028, #10995, #2609, #15197, #8112, #20680, #23575, #21135, #10969, #21332, #1231, #21228 ) ) ;
#21158 = ADVANCED_FACE ( 'NONE', ( #23677 ), #21982, .T. ) ;
#21159 = CARTESIAN_POINT ( 'NONE',  ( -0.1527521626045862113, -0.4420638983541222422, 0.4298724737630855164 ) ) ;
#21160 = CARTESIAN_POINT ( 'NONE',  ( 1.910449006669871087E-17, 0.3097222222222218435, -0.3119999999999999996 ) ) ;
#21161 = CARTESIAN_POINT ( 'NONE',  ( 0.2206173157302027676, 0.05972222207048929338, 0.2206173157302028787 ) ) ;
#21162 = CARTESIAN_POINT ( 'NONE',  ( 0.3033084913416829176, 5.145647145552547208, 0.01295876866797208288 ) ) ;
#21163 = AXIS2_PLACEMENT_3D ( 'NONE', #14780, #15131, #4140 ) ;
#21164 = CARTESIAN_POINT ( 'NONE',  ( -5.731347020009612645E-17, 0.1638888887371559577, 0.3119999999999999996 ) ) ;
#21165 = CARTESIAN_POINT ( 'NONE',  ( -5.731347020009612645E-17, 0.3305555554038226429, 0.3119999999999999996 ) ) ;
#21166 = DIRECTION ( 'NONE',  ( -0.000000000000000000, -1.000000000000000000, -0.000000000000000000 ) ) ;
#21167 = EDGE_LOOP ( 'NONE', ( #23003, #13116, #14156, #13824, #19711, #5126 ) ) ;
#21168 = CARTESIAN_POINT ( 'NONE',  ( -0.2764156081756484196, -0.1144950937579609362, 0.2029166666666694652 ) ) ;
#21169 = CARTESIAN_POINT ( 'NONE',  ( -0.2819296736111110979, 0.1187499999241333620, -3.452642723725051716E-17 ) ) ;
#21170 = CARTESIAN_POINT ( 'NONE',  ( 0.1954553509668047195, 0.1954553509668046085, 0.4633333333333381487 ) ) ;
#21171 = CARTESIAN_POINT ( 'NONE',  ( -1.726321361862525858E-17, 4.686194444520309865, -0.2819296736111110979 ) ) ;
#21172 = CARTESIAN_POINT ( 'NONE',  ( 2.986000000000000210, 2.740000000000000213, -2.541000000000000369 ) ) ;
#21173 = CARTESIAN_POINT ( 'NONE',  ( -0.1993543840281266910, 4.623694444520309865, -0.1993543840281266910 ) ) ;
#21174 = CARTESIAN_POINT ( 'NONE',  ( -0.001112167594266136794, 4.154976392104846816, -0.3119983012180029269 ) ) ;
#21175 = ADVANCED_FACE ( 'NONE', ( #10542 ), #18332, .T. ) ;
#21176 = CARTESIAN_POINT ( 'NONE',  ( 0.3124999999999999445, -0.1294417382415923856, 0.3626388888888927853 ) ) ;
#21177 = CARTESIAN_POINT ( 'NONE',  ( -0.0003315323776482123944, 4.715469205126314599E-18, 0.3725069824736144675 ) ) ;
#21178 = DIRECTION ( 'NONE',  ( 0.000000000000000000, -1.000000000000000000, 0.000000000000000000 ) ) ;
#21179 = CARTESIAN_POINT ( 'NONE',  ( -0.2206173157302027676, 4.224388888888888083, 0.2206173157302028787 ) ) ;
#21180 = CARTESIAN_POINT ( 'NONE',  ( 0.2206173157302027954, 5.148000000151732536, -0.2206173157302028232 ) ) ;
#21181 = CARTESIAN_POINT ( 'NONE',  ( 0.2828693099792405352, 4.978340185095941450, -0.1368988876663677356 ) ) ;
#21182 = ORIENTED_EDGE ( 'NONE', *, *, #8297, .T. ) ;
#21183 = CARTESIAN_POINT ( 'NONE',  ( 0.1337988207375339911, 4.575549332303573635, 0.2837483186149677983 ) ) ;
#21184 = VERTEX_POINT ( 'NONE', #4791 ) ;
#21185 = PRODUCT_DEFINITION ( 'UNKNOWN', '', #9980, #21425 ) ;
#21186 = AXIS2_PLACEMENT_3D ( 'NONE', #4016, #18532, #15240 ) ;
#21187 = CARTESIAN_POINT ( 'NONE',  ( 0.3124999999999989453, -0.1294417382415934403, 0.09180555555555759695 ) ) ;
#21188 = DESIGN_CONTEXT ( 'detailed design', #1411, 'design' ) ;
#21189 = CARTESIAN_POINT ( 'NONE',  ( 0.3110870456949443863, 4.140046527910736351, 0.03488342758349934764 ) ) ;
#21190 = CARTESIAN_POINT ( 'NONE',  ( -0.2230971623002954152, -0.2230971623002953874, 0.01715277777777927601 ) ) ;
#21191 = CARTESIAN_POINT ( 'NONE',  ( -0.5116234456863466562, 0.9548081934128058723, 2.754369331946250110 ) ) ;
#21192 = CARTESIAN_POINT ( 'NONE',  ( -0.2233192592356399442, 0.09017857133102905043, -0.3073725909049500049 ) ) ;
#21193 = CARTESIAN_POINT ( 'NONE',  ( 0.1993543840281266355, 0.4729166665908000611, 0.1993543840281267465 ) ) ;
#21194 = CARTESIAN_POINT ( 'NONE',  ( -0.03908633756214337229, 5.206640035683666845, 0.2793782410116296688 ) ) ;
#21195 = CARTESIAN_POINT ( 'NONE',  ( 0.3613381517857143232, 0.008035714188171892355, 0.1174058825155741975 ) ) ;
#21196 = CARTESIAN_POINT ( 'NONE',  ( 0.3119999999999999996, 0.5215277777777775903, -0.1292346314604056468 ) ) ;
#21197 = DIRECTION ( 'NONE',  ( 0.000000000000000000, 1.000000000000000000, 0.000000000000000000 ) ) ;
#21198 = CONICAL_SURFACE ( 'NONE', #4054, 0.2109499999999998043, 1.029744258676653645 ) ;
#21199 = EDGE_LOOP ( 'NONE', ( #13446, #905, #3591, #16400 ) ) ;
#21200 = CARTESIAN_POINT ( 'NONE',  ( -0.2467709493912808305, 5.110806576942171553, 0.1882333731734037174 ) ) ;
#21201 = CARTESIAN_POINT ( 'NONE',  ( -0.003269416932270002331, 0.5491886443627419512, 0.04193793378272828165 ) ) ;
#21202 = DIRECTION ( 'NONE',  ( 1.000000000000000000, -0.000000000000000000, 1.224646799147353207E-16 ) ) ;
#21203 = CARTESIAN_POINT ( 'NONE',  ( -0.3119999999999999996, 0.3756944444444441089, -0.1292346314604056745 ) ) ;
#21204 = CARTESIAN_POINT ( 'NONE',  ( 5.731347020009612645E-17, 5.009111111111110404, 0.3119999999999999996 ) ) ;
#21205 = ADVANCED_FACE ( 'NONE', ( #18087 ), #17854, .T. ) ;
#21206 = CARTESIAN_POINT ( 'NONE',  ( -0.1167790944451423535, 3.877166666742531742, 0.2819296736111110424 ) ) ;
#21207 = CARTESIAN_POINT ( 'NONE',  ( -0.2206173157302027676, 3.835499999999998799, 0.2206173157302028787 ) ) ;
#21208 = CARTESIAN_POINT ( 'NONE',  ( -0.04345060704004083396, 0.5161796576942548898, 0.4013192973759855953 ) ) ;
#21209 = CARTESIAN_POINT ( 'NONE',  ( 0.07179678270565797993, 4.819533739383511595, -0.3060367993099030737 ) ) ;
#21210 = VECTOR ( 'NONE', #5882, 39.37007874015748143 ) ;
#21211 = EDGE_LOOP ( 'NONE', ( #1845, #1730, #7565, #23665, #8155, #17715, #12485, #793, #17597, #8100, #7008, #7805 ) ) ;
#21212 = ORIENTED_EDGE ( 'NONE', *, *, #612, .T. ) ;
#21213 = CARTESIAN_POINT ( 'NONE',  ( -0.1571291158571934687, 3.992938027066821771, -0.2726213563812835972 ) ) ;
#21214 = CARTESIAN_POINT ( 'NONE',  ( 0.1167790944451422702, 4.724388888964754507, -0.2819296736111110424 ) ) ;
#21215 = EDGE_CURVE ( 'NONE', #23261, #16762, #14441, .T. ) ;
#21216 = CARTESIAN_POINT ( 'NONE',  ( 0.1650495903302502676, 0.4585922144775744780, 0.07156651416104257979 ) ) ;
#21217 = CARTESIAN_POINT ( 'NONE',  ( 0.4593750000000003664, -0.2760455974562899817, 0.3779506566538943235 ) ) ;
#21218 = CONICAL_SURFACE ( 'NONE', #11089, 0.2041999999999999926, 0.7853981633974563836 ) ;
#21219 = SECURITY_CLASSIFICATION_LEVEL ( 'unclassified' ) ;
#21220 = CARTESIAN_POINT ( 'NONE',  ( 0.000000000000000000, 0.9040586665785882436, 1.048989065017511546 ) ) ;
#21221 = CARTESIAN_POINT ( 'NONE',  ( -0.09435543239133792337, 1.041821957232212270, -2.854670964936879329 ) ) ;
#21222 = CARTESIAN_POINT ( 'NONE',  ( 0.1993543840281267465, 4.276472222298088433, 0.1993543840281266633 ) ) ;
#21223 = CALENDAR_DATE ( 2026, 7, 10 ) ;
#21224 = CARTESIAN_POINT ( 'NONE',  ( -0.2206173157302028232, 4.877166666666665762, -0.2206173157302028232 ) ) ;
#21225 = CARTESIAN_POINT ( 'NONE',  ( 0.2764156081756484196, -5.077672346800151106E-17, 0.1230555555555576941 ) ) ;
#21226 = CC_DESIGN_SECURITY_CLASSIFICATION ( #22007, ( #8363 ) ) ;
#21227 = DIRECTION ( 'NONE',  ( -0.000000000000000000, -1.000000000000000000, -0.000000000000000000 ) ) ;
#21228 = ORIENTED_EDGE ( 'NONE', *, *, #843, .T. ) ;
#21229 = CARTESIAN_POINT ( 'NONE',  ( -0.1167790944451422702, 0.5111111110352446474, -0.2819296736111110424 ) ) ;
#21230 = CARTESIAN_POINT ( 'NONE',  ( 0.4800173678775926378, 0.1715347676940233990, 0.06110638151955335995 ) ) ;
#21231 = CARTESIAN_POINT ( 'NONE',  ( 0.3120000000000000551, 4.463972222222222008, 0.1292346314604056190 ) ) ;
#21232 = CARTESIAN_POINT ( 'NONE',  ( 2.986000000000000210, 0.05000000000000028727, -2.591000000000000636 ) ) ;
#21233 = CARTESIAN_POINT ( 'NONE',  ( 0.2230971623002954429, 0.2230971623002953319, 0.2636805555555586378 ) ) ;
#21234 = ORIENTED_EDGE ( 'NONE', *, *, #8159, .F. ) ;
#21235 = CARTESIAN_POINT ( 'NONE',  ( 0.2209708691207961651, 0.2209708691207959985, 0.03972222222222351884 ) ) ;
#21236 = ADVANCED_FACE ( 'NONE', ( #15377 ), #22924, .F. ) ;
#21237 = CARTESIAN_POINT ( 'NONE',  ( -0.02548689453205812278, 3.766744744258326172, -0.3109991600399485412 ) ) ;
#21238 = CARTESIAN_POINT ( 'NONE',  ( 1.726321361862525858E-17, 0.4381944443685778512, -0.2819296736111110979 ) ) ;
#21239 = CARTESIAN_POINT ( 'NONE',  ( -0.2819296736111110979, 0.2888888888130223265, 0.1167790944451422425 ) ) ;
#21240 = ADVANCED_FACE ( 'NONE', ( #13439 ), #2569, .T. ) ;
#21241 = EDGE_CURVE ( 'NONE', #960, #14698, #18706, .T. ) ;
#21242 = CARTESIAN_POINT ( 'NONE',  ( 0.2819296736111110979, 4.061194444520309865, -3.452642723725051716E-17 ) ) ;
#21243 = CARTESIAN_POINT ( 'NONE',  ( 0.2472135954999579721, 0.4017857140906295199, -0.3402603233408159622 ) ) ;
#21244 = CIRCLE ( 'NONE', #15397, 0.2041999999999999926 ) ;
#21245 = CARTESIAN_POINT ( 'NONE',  ( -0.1167790944451423535, 4.543833333409199149, 0.2819296736111110424 ) ) ;
#21246 = CARTESIAN_POINT ( 'NONE',  ( 0.2710853860383645730, 5.083076204145490884, -0.1547793690661009858 ) ) ;
#21247 = VERTEX_POINT ( 'NONE', #13792 ) ;
#21248 = CARTESIAN_POINT ( 'NONE',  ( 0.1292346314604031765, 4.033416666666667538, -0.3120000000000024420 ) ) ;
#21249 = CARTESIAN_POINT ( 'NONE',  ( 0.3119999999999999996, 3.863277777929509771, -3.820898013339742174E-17 ) ) ;
#21250 = ADVANCED_FACE ( 'NONE', ( #15618 ), #17322, .T. ) ;
#21251 = CC_DESIGN_SECURITY_CLASSIFICATION ( #6827, ( #582 ) ) ;
#21252 = CARTESIAN_POINT ( 'NONE',  ( 0.1541993830832357193, -0.2301090524147265115, 0.3880822748423152224 ) ) ;
#21253 = CARTESIAN_POINT ( 'NONE',  ( 0.1125312330130331800, 0.03242967361111057795, 0.2589088460590495688 ) ) ;
#21254 = PERSON_AND_ORGANIZATION ( #15518, #2538 ) ;
#21255 = CIRCLE ( 'NONE', #11130, 1.015181661097394050 ) ;
#21256 = CARTESIAN_POINT ( 'NONE',  ( 0.2229532752983993393, 0.1767350293216415902, 0.3955450596469902713 ) ) ;
#21257 = CARTESIAN_POINT ( 'NONE',  ( -0.2919173025508979280, 4.998982188319265774, -0.1102035603291813132 ) ) ;
#21258 = ORIENTED_EDGE ( 'NONE', *, *, #4587, .T. ) ;
#21259 = CARTESIAN_POINT ( 'NONE',  ( 1.910449006669871087E-17, 0.6361111109593781121, -0.3119999999999999996 ) ) ;
#21260 = ORIENTED_EDGE ( 'NONE', *, *, #11057, .T. ) ;
#21261 = LINE ( 'NONE', #17244, #775 ) ;
#21262 = CARTESIAN_POINT ( 'NONE',  ( 0.03174294256098306871, 3.006956914082103083, -0.8805872809959580660 ) ) ;
#21263 = CARTESIAN_POINT ( 'NONE',  ( -0.2233192592356399442, 0.2330357141881718441, -0.3073725909049500049 ) ) ;
#21264 = DIRECTION ( 'NONE',  ( 1.707404996040164512E-16, 0.000000000000000000, -1.000000000000000000 ) ) ;
#21265 = CC_DESIGN_APPROVAL ( #8209, ( #7632 ) ) ;
#21266 = CARTESIAN_POINT ( 'NONE',  ( -0.1116596296178200276, 0.4187499999024575370, 0.3436530038418508792 ) ) ;
#21267 = CARTESIAN_POINT ( 'NONE',  ( -0.2491085460084383196, 4.662980843054849167, -0.1922337267564872276 ) ) ;
#21268 = CARTESIAN_POINT ( 'NONE',  ( -0.1993543840281266910, 3.845916666742532186, -0.1993543840281266910 ) ) ;
#21269 = CARTESIAN_POINT ( 'NONE',  ( 0.2596226291738499281, 5.035194357586231462, -0.1734927606623648810 ) ) ;
#21270 = DIRECTION ( 'NONE',  ( -0.000000000000000000, 1.000000000000000000, -0.000000000000000000 ) ) ;
#21271 = CARTESIAN_POINT ( 'NONE',  ( -5.731347020009612645E-17, 0.3305555554038226429, 0.3119999999999999996 ) ) ;
#21272 = CARTESIAN_POINT ( 'NONE',  ( -0.1292346314604057023, 4.512583333485064685, 0.3119999999999998885 ) ) ;
#21273 = EDGE_CURVE ( 'NONE', #7634, #19443, #15252, .T. ) ;
#21274 = CARTESIAN_POINT ( 'NONE',  ( -1.726321361862525858E-17, 4.686194444520309865, -0.2819296736111110979 ) ) ;
#21275 = ORIENTED_EDGE ( 'NONE', *, *, #10878, .F. ) ;
#21276 = CARTESIAN_POINT ( 'NONE',  ( 0.2819296736111110979, 4.158416666742532186, -3.452642723725051716E-17 ) ) ;
#21277 = ORIENTED_EDGE ( 'NONE', *, *, #19502, .F. ) ;
#21278 = CARTESIAN_POINT ( 'NONE',  ( 0.2923287055106771337, 0.2723214284738861291, 0.2123892367102621359 ) ) ;
#21279 = ORIENTED_EDGE ( 'NONE', *, *, #1659, .T. ) ;
#21280 = ORGANIZATION ( 'NAUO-ORG7', 'UNSPECIFIED', 'UNSPECIFIED' ) ;
#21281 = ORIENTED_EDGE ( 'NONE', *, *, #17202, .T. ) ;
#21282 = PERSON_AND_ORGANIZATION ( #15518, #2538 ) ;
#21283 = LINE ( 'NONE', #13970, #21601 ) ;
#21284 = CARTESIAN_POINT ( 'NONE',  ( -0.3394572874457115752, 3.700000000000000622, 0.09499999999999993172 ) ) ;
#21285 = ORIENTED_EDGE ( 'NONE', *, *, #18365, .F. ) ;
#21286 = DIRECTION ( 'NONE',  ( -1.177540334020096294E-17, 0.2588190451025213501, -0.9659258262890680902 ) ) ;
#21287 = CARTESIAN_POINT ( 'NONE',  ( 0.1844455389852084348, 5.136728975353069160, 0.2436424482298817917 ) ) ;
#21288 = CARTESIAN_POINT ( 'NONE',  ( 0.1294417382415921358, -0.3125000000000002220, -0.08180555555555486802 ) ) ;
#21289 = CARTESIAN_POINT ( 'NONE',  ( 0.4687500000000002776, 0.2598076211353318454, 0.06112444011295372487 ) ) ;
#21290 = CARTESIAN_POINT ( 'NONE',  ( 0.1167790944451423119, 0.1013888888130222571, -0.2819296736111110979 ) ) ;
#21291 = CARTESIAN_POINT ( 'NONE',  ( -0.2764156081756484196, 0.1144950937579609918, 0.08486111111111295513 ) ) ;
#21292 = ORIENTED_EDGE ( 'NONE', *, *, #3456, .F. ) ;
#21293 = CARTESIAN_POINT ( 'NONE',  ( 0.000000000000000000, 3.700000000000000622, 0.000000000000000000 ) ) ;
#21294 = CARTESIAN_POINT ( 'NONE',  ( 0.1167790944451422702, 4.668833333409200037, -0.2819296736111110424 ) ) ;
#21295 = CARTESIAN_POINT ( 'NONE',  ( 0.4592359490081627804, -0.08899061577413990010, 0.4306447894611612481 ) ) ;
#21296 = CARTESIAN_POINT ( 'NONE',  ( -0.1577217838551094042, 0.2181752645060030527, -1.222675257892397838 ) ) ;
#21297 = CARTESIAN_POINT ( 'NONE',  ( 0.1940838408004180171, 3.748630699786517528, -0.2346081964820543042 ) ) ;
#21298 = DIRECTION ( 'NONE',  ( -0.5000000000000001110, 0.8660254037844385966, 0.000000000000000000 ) ) ;
#21299 = B_SPLINE_CURVE_WITH_KNOTS ( 'NONE', 3,
 ( #22867, #13621, #21040, #15199 ),
 .UNSPECIFIED., .F., .F.,
 ( 4, 4 ),
 ( 1.008999589182314829E-06, 0.001469413801632195879 ),
 .UNSPECIFIED. ) ;
#21300 = CARTESIAN_POINT ( 'NONE',  ( -0.3119999999999998885, 4.220916666666665762, 0.1292346314604058410 ) ) ;
#21301 = EDGE_CURVE ( 'NONE', #9027, #20864, #10017, .T. ) ;
#21302 = CARTESIAN_POINT ( 'NONE',  ( 0.3119999999999999996, 5.200083333485065573, -0.1292346314604056745 ) ) ;
#21303 = CARTESIAN_POINT ( 'NONE',  ( 0.09556577126599200001, 4.963224787294483242, 0.2971471245525674210 ) ) ;
#21304 = CARTESIAN_POINT ( 'NONE',  ( -0.4366234456863467006, 0.9548081934128058723, 2.592671479769666387 ) ) ;
#21305 = VECTOR ( 'NONE', #17214, 39.37007874015748143 ) ;
#21306 = CARTESIAN_POINT ( 'NONE',  ( 0.000000000000000000, 0.4202679491924311561, 0.2499999999999999722 ) ) ;
#21307 = ORIENTED_EDGE ( 'NONE', *, *, #3752, .F. ) ;
#21308 =( BOUNDED_CURVE ( )  B_SPLINE_CURVE ( 2, ( #20256, #12469, #10631, #18303, #12718, #5370, #16479, #12959, #12837 ),
 .UNSPECIFIED., .F., .T. ) 
 B_SPLINE_CURVE_WITH_KNOTS ( ( 3, 2, 2, 2, 3 ),
 ( 0.4196428571428572063, 0.4241071428571429047, 0.4285714285714286031, 0.4330357142857143571, 0.4375000000000000555 ),
 .UNSPECIFIED. ) 
 CURVE ( )  GEOMETRIC_REPRESENTATION_ITEM ( )  RATIONAL_B_SPLINE_CURVE ( ( 0.9999999999999990008, 0.9238795325112877377, 1.000000000000000000, 0.9238795325112867385, 1.000000000000000000, 0.9238795325112867385, 1.000000000000000000, 0.9238795325112857393, 1.000000000000000888 ) ) 
 REPRESENTATION_ITEM ( '' )  );
#21309 =( BOUNDED_CURVE ( )  B_SPLINE_CURVE ( 2, ( #7702, #18797, #15267, #3806, #9534, #20984, #22815, #2092, #5755 ),
 .UNSPECIFIED., .F., .T. ) 
 B_SPLINE_CURVE_WITH_KNOTS ( ( 3, 2, 2, 2, 3 ),
 ( 0.4375000000000000555, 0.4479166666666667407, 0.4583333333333333703, 0.4687500000000000555, 0.4791666666666667407 ),
 .UNSPECIFIED. ) 
 CURVE ( )  GEOMETRIC_REPRESENTATION_ITEM ( )  RATIONAL_B_SPLINE_CURVE ( ( 0.9999999999999995559, 0.9238795325112871826, 1.000000000000000000, 0.9238795325112867385, 1.000000000000000000, 0.9238795325112867385, 1.000000000000000000, 0.9238795325112862944, 1.000000000000000444 ) ) 
 REPRESENTATION_ITEM ( '' )  );
#21310 = CARTESIAN_POINT ( 'NONE',  ( 0.04847343760161313547, 4.684065114164263299, 0.3082221411203268646 ) ) ;
#21311 = DIRECTION ( 'NONE',  ( -1.000000000000000000, 0.000000000000000000, 0.000000000000000000 ) ) ;
#21312 = CARTESIAN_POINT ( 'NONE',  ( -0.3155070326520293400, 0.1306872919485614903, -0.04881944444444345776 ) ) ;
#21313 = LINE ( 'NONE', #8369, #23938 ) ;
#21314 = CARTESIAN_POINT ( 'NONE',  ( 0.3613381517857143232, 0.06160714275960043479, 0.1174058825155742114 ) ) ;
#21315 = VECTOR ( 'NONE', #14492, 39.37007874015748143 ) ;
#21316 = FACE_OUTER_BOUND ( 'NONE', #13472, .T. ) ;
#21317 = CARTESIAN_POINT ( 'NONE',  ( 0.1954553509668046640, -0.1954553509668047195, 0.1161111111111132049 ) ) ;
#21318 = CARTESIAN_POINT ( 'NONE',  ( 0.4784936136544857277, -0.2687202946394928182, 0.04212966708837330432 ) ) ;
#21319 = CARTESIAN_POINT ( 'NONE',  ( 0.009374999999999774139, 0.5358532185916217161, 0.06112444011295372487 ) ) ;
#21320 = CARTESIAN_POINT ( 'NONE',  ( 0.000000000000000000, 5.384999999999999787, 0.000000000000000000 ) ) ;
#21321 = EDGE_LOOP ( 'NONE', ( #3718, #23056, #16000, #15438, #13271, #1072, #9328, #806, #23190 ) ) ;
#21322 = CARTESIAN_POINT ( 'NONE',  ( -0.1379734605153020432, 4.623101557285290042, 0.2798964025940948175 ) ) ;
#21323 = CC_DESIGN_PERSON_AND_ORGANIZATION_ASSIGNMENT ( #71, #3857, ( #12686 ) ) ;
#21324 = CARTESIAN_POINT ( 'NONE',  ( 0.2472135954999579721, 0.1249999999999999306, -0.3402603233408160732 ) ) ;
#21325 = DIRECTION ( 'NONE',  ( -0.000000000000000000, -1.000000000000000000, -0.000000000000000000 ) ) ;
#21326 = CARTESIAN_POINT ( 'NONE',  ( 0.3119999999999998885, 0.5701388888888886397, 0.1292346314604058410 ) ) ;
#21327 = CARTESIAN_POINT ( 'NONE',  ( -0.1292346314604056745, 5.040361111111110404, -0.3119999999999999996 ) ) ;
#21328 = CARTESIAN_POINT ( 'NONE',  ( -0.1993543840281266355, 3.984805555631421470, 0.1993543840281267465 ) ) ;
#21329 = DIRECTION ( 'NONE',  ( -0.000000000000000000, -1.000000000000000000, -0.000000000000000000 ) ) ;
#21330 = DIRECTION ( 'NONE',  ( -0.000000000000000000, -1.000000000000000000, -0.000000000000000000 ) ) ;
#21331 = CARTESIAN_POINT ( 'NONE',  ( 0.2285105464130554875, -9.196729208309095321E-18, 0.2808975190895516838 ) ) ;
#21332 = ORIENTED_EDGE ( 'NONE', *, *, #3456, .T. ) ;
#21333 = VERTEX_POINT ( 'NONE', #15497 ) ;
#21334 = CARTESIAN_POINT ( 'NONE',  ( -0.3125000000000000000, -0.1294417382415921913, -0.04013888888888785672 ) ) ;
#21335 = CARTESIAN_POINT ( 'NONE',  ( 5.178964085587577574E-17, 4.644527777853642903, 0.2819296736111110979 ) ) ;
#21336 = CARTESIAN_POINT ( 'NONE',  ( 0.2775113281607683446, -0.3935459114639780487, 0.07438423612653363715 ) ) ;
#21337 = DIRECTION ( 'NONE',  ( 0.4999999999999909517, -0.000000000000000000, -0.8660254037844438146 ) ) ;
#21338 = CIRCLE ( 'NONE', #22499, 0.01875000000000002359 ) ;
#21339 = CARTESIAN_POINT ( 'NONE',  ( -0.2742360776603882666, -0.1498359893665253684, -0.1016666666666679597 ) ) ;
#21340 = ADVANCED_FACE ( 'NONE', ( #9892 ), #18915, .T. ) ;
#21341 = CARTESIAN_POINT ( 'NONE',  ( -0.1144950937579609779, 0.2764156081756484196, -0.03319444444444354797 ) ) ;
#21342 = CARTESIAN_POINT ( 'NONE',  ( 0.1167790944451422702, 4.016055555631422358, -0.2819296736111110979 ) ) ;
#21343 = COORDINATED_UNIVERSAL_TIME_OFFSET ( 0, 0, .AHEAD. ) ;
#21344 = CARTESIAN_POINT ( 'NONE',  ( 0.3125000000000000000, -5.740531871003217465E-17, -0.07833333333333296344 ) ) ;
#21345 = CARTESIAN_POINT ( 'NONE',  ( 0.2209708691207961095, -0.2209708691207961651, 0.3036111111111144956 ) ) ;
#21346 = CARTESIAN_POINT ( 'NONE',  ( 0.2764156081756484196, -5.077672346800151106E-17, 0.1786111111111136907 ) ) ;
#21347 = CARTESIAN_POINT ( 'NONE',  ( 0.000000000000000000, 0.05000000000000028727, -0.6537512679238876023 ) ) ;
#21348 = CARTESIAN_POINT ( 'NONE',  ( -0.1993543840281267465, 0.07013888881302225708, 0.1993543840281266633 ) ) ;
#21349 = DIRECTION ( 'NONE',  ( -0.5000000000000007772, 0.000000000000000000, -0.8660254037844382635 ) ) ;
#21350 = DIRECTION ( 'NONE',  ( 0.000000000000000000, 1.000000000000000000, 0.000000000000000000 ) ) ;
#21351 = CARTESIAN_POINT ( 'NONE',  ( -0.2209708691207961095, 0.2209708691207961373, -0.001944444444443472510 ) ) ;
#21352 = CARTESIAN_POINT ( 'NONE',  ( 0.3155070326520292290, 0.1306872919485615736, 0.4824305555555604141 ) ) ;
#21353 = EDGE_CURVE ( 'NONE', #6836, #21772, #4390, .T. ) ;
#21354 = ORIENTED_EDGE ( 'NONE', *, *, #4658, .T. ) ;
#21355 = CARTESIAN_POINT ( 'NONE',  ( 0.000000000000000000, 0.3125000000000000000, 0.04666666666666802188 ) ) ;
#21356 = CARTESIAN_POINT ( 'NONE',  ( 0.03174294256098300626, 3.006956914082103083, -0.8805872809959580660 ) ) ;
#21357 = CARTESIAN_POINT ( 'NONE',  ( -0.1993543840281267465, 0.5145833332574667462, 0.1993543840281266633 ) ) ;
#21358 = CARTESIAN_POINT ( 'NONE',  ( 0.2819296736111110424, 0.5319444443685777957, 0.1167790944451424923 ) ) ;
#21359 = CARTESIAN_POINT ( 'NONE',  ( 0.2819296736111110979, 4.168833333409199149, 0.1167790944451422425 ) ) ;
#21360 = AXIS2_PLACEMENT_3D ( 'NONE', #13991, #21419, #19707 ) ;
#21361 = CARTESIAN_POINT ( 'NONE',  ( -0.3613381517857143232, 0.1187499999024576036, -4.425116109941954795E-17 ) ) ;
#21362 = CARTESIAN_POINT ( 'NONE',  ( 0.2819296736111110979, 4.668833333409200037, 0.1167790944451422425 ) ) ;
#21363 = PLANE ( 'NONE',  #24043 ) ;
#21364 = CARTESIAN_POINT ( 'NONE',  ( 0.4000000000000000222, 0.1767857140906294589, 0.000000000000000000 ) ) ;
#21365 = VERTEX_POINT ( 'NONE', #7692 ) ;
#21366 = VERTEX_POINT ( 'NONE', #15140 ) ;
#21367 = CARTESIAN_POINT ( 'NONE',  ( 0.3124999999999993339, 0.1294417382415928297, 0.3765277777777821244 ) ) ;
#21368 = CARTESIAN_POINT ( 'NONE',  ( -0.3119999999999999996, 3.776472222373954413, -0.1292346314604056468 ) ) ;
#21369 = CARTESIAN_POINT ( 'NONE',  ( 0.2742360776605723416, -0.1498359893662102316, 0.4241666666666772390 ) ) ;
#21370 = ORIENTED_EDGE ( 'NONE', *, *, #8118, .T. ) ;
#21371 = CIRCLE ( 'NONE', #3459, 0.09499999999999995948 ) ;
#21372 = APPROVAL_STATUS ( 'not_yet_approved' ) ;
#21373 = ORIENTED_EDGE ( 'NONE', *, *, #21697, .F. ) ;
#21374 = CARTESIAN_POINT ( 'NONE',  ( 0.4057955023597048516, 2.693521551442877193, -0.6418853869074238050 ) ) ;
#21375 = ORIENTED_EDGE ( 'NONE', *, *, #21699, .T. ) ;
#21376 = CARTESIAN_POINT ( 'NONE',  ( 0.2819296736111110424, 0.1638888888130222432, -0.1167790944451423119 ) ) ;
#21377 = ORIENTED_EDGE ( 'NONE', *, *, #13407, .F. ) ;
#21378 = CARTESIAN_POINT ( 'NONE',  ( 0.0007571358743316145218, 4.266035208878255602, -0.3119992139512273166 ) ) ;
#21379 = FACE_OUTER_BOUND ( 'NONE', #15349, .T. ) ;
#21380 = CARTESIAN_POINT ( 'NONE',  ( 0.3137470792316710555, 4.086203903373451851, -0.02617354482465570481 ) ) ;
#21381 = CARTESIAN_POINT ( 'NONE',  ( -0.3613381517857143232, 0.3830357141881717276, -0.1174058825155741004 ) ) ;
#21382 = CARTESIAN_POINT ( 'NONE',  ( -0.3119999999999999996, 4.491749999999999687, -0.1292346314604056468 ) ) ;
#21383 = ADVANCED_FACE ( 'NONE', ( #7923 ), #295, .F. ) ;
#21384 = PLANE ( 'NONE',  #18208 ) ;
#21385 = LINE ( 'NONE', #17725, #8594 ) ;
#21386 = EDGE_LOOP ( 'NONE', ( #20257, #22488, #595, #7851 ) ) ;
#21387 = CARTESIAN_POINT ( 'NONE',  ( -0.1167790944451423535, 5.210500000075866112, 0.2819296736111110424 ) ) ;
#21388 = SPHERICAL_SURFACE ( 'NONE', #8676, 0.3119999999999999996 ) ;
#21389 = DIRECTION ( 'NONE',  ( -0.8320502943378438321, -0.4803844614152618653, -0.2773500981126136300 ) ) ;
#21390 = VECTOR ( 'NONE', #12672, 39.37007874015748854 ) ;
#21391 = CARTESIAN_POINT ( 'NONE',  ( -0.3133020153825915033, 4.780755246673074055, 0.02780367048916862482 ) ) ;
#21392 = CARTESIAN_POINT ( 'NONE',  ( -0.2206173157302027676, 4.564666666818398610, 0.2206173157302028787 ) ) ;
#21393 = CARTESIAN_POINT ( 'NONE',  ( 0.1993543840281267465, 4.720916666742533074, 0.1993543840281266633 ) ) ;
#21394 = EDGE_LOOP ( 'NONE', ( #5538, #14829, #6484, #22970 ) ) ;
#21395 = EDGE_CURVE ( 'NONE', #18107, #6978, #2896, .T. ) ;
#21396 = CARTESIAN_POINT ( 'NONE',  ( -0.2819296736111110424, 4.071611111186976828, -0.1167790944451423119 ) ) ;
#21397 = ADVANCED_FACE ( 'NONE', ( #13267 ), #9590, .F. ) ;
#21398 = EDGE_CURVE ( 'NONE', #9027, #3958, #16544, .T. ) ;
#21399 = APPROVAL_DATE_TIME ( #23211, #17441 ) ;
#21400 = ORIENTED_EDGE ( 'NONE', *, *, #10756, .T. ) ;
#21401 = CARTESIAN_POINT ( 'NONE',  ( -0.4581189881604794678, -0.2644951211353319120, 0.3941886329748524598 ) ) ;
#21402 = CARTESIAN_POINT ( 'NONE',  ( 0.3119999999999998885, 0.4590277777777774237, 0.1292346314604058410 ) ) ;
#21403 = AXIS2_PLACEMENT_3D ( 'NONE', #16748, #29, #7476 ) ;
#21404 = DIRECTION ( 'NONE',  ( -0.000000000000000000, -1.000000000000000000, -0.000000000000000000 ) ) ;
#21405 = DIRECTION ( 'NONE',  ( -0.000000000000000000, -1.000000000000000000, -0.000000000000000000 ) ) ;
#21406 = CARTESIAN_POINT ( 'NONE',  ( -0.4687500000000004441, 0.2174757758404408658, 0.3901708077920437723 ) ) ;
#21407 = ADVANCED_FACE ( 'NONE', ( #15319 ), #9543, .T. ) ;
#21408 = DIRECTION ( 'NONE',  ( 0.000000000000000000, 0.000000000000000000, -1.000000000000000000 ) ) ;
#21409 = CARTESIAN_POINT ( 'NONE',  ( 0.2819296736111110424, 0.1430555554796889284, 0.1167790944451424923 ) ) ;
#21410 = CARTESIAN_POINT ( 'NONE',  ( -0.2764156081756484196, -0.1144950937579609362, -0.01930555555555453148 ) ) ;
#21411 = CARTESIAN_POINT ( 'NONE',  ( 0.000000000000000000, 0.000000000000000000, 0.000000000000000000 ) ) ;
#21412 = CARTESIAN_POINT ( 'NONE',  ( -0.1167790944451423257, 4.509111111186976828, -0.2819296736111110424 ) ) ;
#21413 = CARTESIAN_POINT ( 'NONE',  ( -0.1167790944451423535, 5.196611111186976828, 0.2819296736111110979 ) ) ;
#21414 = CARTESIAN_POINT ( 'NONE',  ( -0.2982593250668997276, 0.5727001298589282641, -1.097990058363176535 ) ) ;
#21415 = CARTESIAN_POINT ( 'NONE',  ( -0.3125000000000000000, 1.913510623667739771E-17, -0.09916666666666609786 ) ) ;
#21416 = CARTESIAN_POINT ( 'NONE',  ( 0.3119999999999999996, 0.4590277776260448528, -0.1292346314604056468 ) ) ;
#21417 = CARTESIAN_POINT ( 'NONE',  ( -0.1292346314604057023, 4.172305555555555046, 0.3119999999999998885 ) ) ;
#21418 = CARTESIAN_POINT ( 'NONE',  ( 0.2383741534419201169, 5.072285808806758389, 0.2028604780184855572 ) ) ;
#21419 = DIRECTION ( 'NONE',  ( 0.000000000000000000, 1.000000000000000000, 0.000000000000000000 ) ) ;
#21420 = AXIS2_PLACEMENT_3D ( 'NONE', #13973, #4693, #12161 ) ;
#21421 = AXIS2_PLACEMENT_3D ( 'NONE', #11374, #2229, #16858 ) ;
#21422 = CARTESIAN_POINT ( 'NONE',  ( 0.4224968603155544455, 0.2973372013303175465, 0.07046346805502540223 ) ) ;
#21423 = CARTESIAN_POINT ( 'NONE',  ( -1.562282291722813840E-15, -0.000000000000000000, -2.540999999999999037 ) ) ;
#21424 = CARTESIAN_POINT ( 'NONE',  ( -0.3120460406368502637, 4.889979835822584775, -0.04045770392581769098 ) ) ;
#21425 = DESIGN_CONTEXT ( 'detailed design', #22126, 'design' ) ;
#21426 = CARTESIAN_POINT ( 'NONE',  ( 0.4805453593044337612, -0.2624503992731451185, 0.04271845132551427976 ) ) ;
#21427 = CARTESIAN_POINT ( 'NONE',  ( -0.1306872919485614903, 0.3155070326520293400, -0.0002083333333319594999 ) ) ;
#21428 = CARTESIAN_POINT ( 'NONE',  ( 0.1966284714786247223, 0.4277423764267400674, 0.07944889038204620835 ) ) ;
#21429 = ADVANCED_FACE ( 'NONE', ( #552 ), #316, .T. ) ;
#21430 = CARTESIAN_POINT ( 'NONE',  ( 0.04084074131989445106, 3.820513810923966691, -0.3119999999999996110 ) ) ;
#21431 = ADVANCED_FACE ( 'NONE', ( #5687 ), #17148, .F. ) ;
#21432 = CONICAL_SURFACE ( 'NONE', #19863, 0.2500000000000000555, 0.5235987755984723435 ) ;
#21433 = CARTESIAN_POINT ( 'NONE',  ( -0.2923287055106771337, 0.3223214284738861735, 0.2123892367102619971 ) ) ;
#21434 = AXIS2_PLACEMENT_3D ( 'NONE', #10532, #12372, #8323 ) ;
#21435 = CARTESIAN_POINT ( 'NONE',  ( 0.2764156081756483641, 0.1144950937579610056, -0.04013888888888804407 ) ) ;
#21436 = LINE ( 'NONE', #10353, #14705 ) ;
#21437 = FACE_OUTER_BOUND ( 'NONE', #16730, .T. ) ;
#21438 = CARTESIAN_POINT ( 'NONE',  ( 0.000000000000000000, 0.2764156081756484196, 0.3036111111111146621 ) ) ;
#21439 = CARTESIAN_POINT ( 'NONE',  ( -0.04998852818392456737, 4.600835773807371964, -0.3081328456724486964 ) ) ;
#21440 = CARTESIAN_POINT ( 'NONE',  ( -1.399103805173478513E-17, 0.4635611116728546865, -1.084197934689580034 ) ) ;
#21441 = DIRECTION ( 'NONE',  ( -3.642463991552349380E-15, -0.2142211582677920889, -0.9767851838303064360 ) ) ;
#21442 = CARTESIAN_POINT ( 'NONE',  ( 0.2206173157302028232, 0.3583333333333329485, -0.2206173157302028232 ) ) ;
#21443 = CARTESIAN_POINT ( 'NONE',  ( 0.3119999999999999996, 5.019527777777777366, 0.1292346314604056190 ) ) ;
#21444 = CARTESIAN_POINT ( 'NONE',  ( 0.1993543840281266633, 4.220916666742532186, -0.1993543840281266910 ) ) ;
#21445 = CARTESIAN_POINT ( 'NONE',  ( 0.2819296736111110979, 3.950083333409199149, -3.452642723725051716E-17 ) ) ;
#21446 =( BOUNDED_CURVE ( )  B_SPLINE_CURVE ( 2, ( #10867, #13189, #1945, #18414, #16831, #14647, #20603, #20125, #18296 ),
 .UNSPECIFIED., .F., .T. ) 
 B_SPLINE_CURVE_WITH_KNOTS ( ( 3, 2, 2, 2, 3 ),
 ( 0.3482142857142856429, 0.3526785714285713969, 0.3571428571428570953, 0.3616071428571428492, 0.3660714285714285476 ),
 .UNSPECIFIED. ) 
 CURVE ( )  GEOMETRIC_REPRESENTATION_ITEM ( )  RATIONAL_B_SPLINE_CURVE ( ( 1.000000000000000888, 0.9238795325112857393, 1.000000000000000000, 0.9238795325112867385, 1.000000000000000000, 0.9238795325112867385, 1.000000000000000000, 0.9238795325112867385, 1.000000000000000000 ) ) 
 REPRESENTATION_ITEM ( '' )  );
#21447 = DIRECTION ( 'NONE',  ( -0.000000000000000000, -0.000000000000000000, -1.000000000000000000 ) ) ;
#21448 = CARTESIAN_POINT ( 'NONE',  ( -0.2534589807566942632, 0.3949312665968688352, 0.4181462219997566510 ) ) ;
#21449 = CARTESIAN_POINT ( 'NONE',  ( 0.3233240115537838744, 3.229549314084639149E-17, 0.1617550376952779367 ) ) ;
#21450 =( BOUNDED_CURVE ( )  B_SPLINE_CURVE ( 2, ( #9038, #10875, #7095, #14533, #11113, #21955, #16483 ),
 .UNSPECIFIED., .F., .F. ) 
 B_SPLINE_CURVE_WITH_KNOTS ( ( 3, 2, 2, 3 ),
 ( 0.9642857142857143016, 0.9714285714285714191, 0.9857142857142857650, 1.000000000000000000 ),
 .UNSPECIFIED. ) 
 CURVE ( )  GEOMETRIC_REPRESENTATION_ITEM ( )  RATIONAL_B_SPLINE_CURVE ( ( 0.9755282581475768211, 0.9755282581475768211, 1.000000000000000000, 0.9510565162951535312, 1.000000000000000000, 0.9510565162951535312, 1.000000000000000000 ) ) 
 REPRESENTATION_ITEM ( '' )  );
#21451 = VERTEX_POINT ( 'NONE', #7515 ) ;
#21452 = ORIENTED_EDGE ( 'NONE', *, *, #20904, .T. ) ;
#21453 = CARTESIAN_POINT ( 'NONE',  ( 0.4875000000000002665, 0.2598076211353318454, 0.06112444011295372487 ) ) ;
#21454 = CARTESIAN_POINT ( 'NONE',  ( 0.2819296736111110424, 4.439666666742532186, -0.1167790944451423396 ) ) ;
#21455 = DIRECTION ( 'NONE',  ( 0.5000000000000008882, 0.000000000000000000, 0.8660254037844380415 ) ) ;
#21456 = VECTOR ( 'NONE', #17790, 39.37007874015748143 ) ;
#21457 = DATE_AND_TIME ( #14026, #8753 ) ;
#21458 = CARTESIAN_POINT ( 'NONE',  ( -0.4687500000000003886, -0.04413379556123714353, 0.09139253360868644649 ) ) ;
#21459 = CARTESIAN_POINT ( 'NONE',  ( -0.1954553509668046640, 0.1954553509668046918, -0.08527777777777728607 ) ) ;
#21460 = CARTESIAN_POINT ( 'NONE',  ( 0.2819296736111111534, 4.002166666742532186, 0.1167790944451422563 ) ) ;
#21461 = CARTESIAN_POINT ( 'NONE',  ( -0.3119999999999999996, 0.3756944444444441089, -0.1292346314604056745 ) ) ;
#21462 = DIRECTION ( 'NONE',  ( -0.000000000000000000, 1.000000000000000000, -0.000000000000000000 ) ) ;
#21463 = CARTESIAN_POINT ( 'NONE',  ( 0.1954553509668046640, -0.1954553509668047195, 0.1161111111111132049 ) ) ;
#21464 = CARTESIAN_POINT ( 'NONE',  ( -0.3613381517857143232, -0.02767857152611381821, -0.1174058825155741004 ) ) ;
#21465 = CARTESIAN_POINT ( 'NONE',  ( -5.178964085587577574E-17, 0.1326388888130222710, 0.2819296736111110979 ) ) ;
#21466 = CARTESIAN_POINT ( 'NONE',  ( 0.4796773874647223823, 0.08638538962819194977, 0.07156402152810012463 ) ) ;
#21467 = CARTESIAN_POINT ( 'NONE',  ( -0.1292346314604056190, 0.4243055555555552139, -0.3119999999999999996 ) ) ;
#21468 = CARTESIAN_POINT ( 'NONE',  ( -0.06335377612981472895, 0.1339733671981016006, -0.3999999999999999667 ) ) ;
#21469 = DIRECTION ( 'NONE',  ( -0.000000000000000000, -1.000000000000000000, -0.000000000000000000 ) ) ;
#21470 = CARTESIAN_POINT ( 'NONE',  ( -0.3155070326520293400, 0.1306872919485614903, 0.2810416666666698537 ) ) ;
#21471 = ORIENTED_EDGE ( 'NONE', *, *, #21969, .F. ) ;
#21472 = DIRECTION ( 'NONE',  ( 0.000000000000000000, 0.000000000000000000, -1.000000000000000000 ) ) ;
#21473 = DIRECTION ( 'NONE',  ( 0.000000000000000000, 0.000000000000000000, 1.000000000000000000 ) ) ;
#21474 = CARTESIAN_POINT ( 'NONE',  ( 1.910449006669871087E-17, 0.4138888887371559577, -0.3119999999999999996 ) ) ;
#21475 = CARTESIAN_POINT ( 'NONE',  ( -0.2819296736111110979, 0.4555555554796890116, 0.1167790944451422425 ) ) ;
#21476 = CARTESIAN_POINT ( 'NONE',  ( 0.2819296736111110424, 4.064666666742532186, -0.1167790944451423396 ) ) ;
#21477 = CARTESIAN_POINT ( 'NONE',  ( -0.2233192592356399442, 0.03660714275960045422, -0.3073725909049500049 ) ) ;
#21478 = CARTESIAN_POINT ( 'NONE',  ( -0.1167790944451423257, 4.689666666742532186, -0.2819296736111110424 ) ) ;
#21479 = CARTESIAN_POINT ( 'NONE',  ( 0.2755744112216236830, 5.134589151667465323, -0.1342242742989331605 ) ) ;
#21480 = CARTESIAN_POINT ( 'NONE',  ( 0.3236067977499790249, 0.1839285712334866041, -0.2351141009169892826 ) ) ;
#21481 = VERTEX_POINT ( 'NONE', #5920 ) ;
#21482 = EDGE_CURVE ( 'NONE', #16231, #20833, #21299, .T. ) ;
#21483 = CARTESIAN_POINT ( 'NONE',  ( 0.2206173157302027954, 3.925777777929509771, -0.2206173157302028232 ) ) ;
#21484 = CARTESIAN_POINT ( 'NONE',  ( 2.055580586463031434, 2.740000000000000213, -2.936000000000001720 ) ) ;
#21485 = APPROVAL ( #16126, 'UNSPECIFIED' ) ;
#21486 = ORIENTED_EDGE ( 'NONE', *, *, #20086, .F. ) ;
#21487 = CARTESIAN_POINT ( 'NONE',  ( -0.2819296736111110424, 4.856333333409198261, 0.1167790944451424923 ) ) ;
#21488 = PERSON_AND_ORGANIZATION_ROLE ( 'design_owner' ) ;
#21489 = ORIENTED_EDGE ( 'NONE', *, *, #20955, .T. ) ;
#21490 = CARTESIAN_POINT ( 'NONE',  ( -0.3091906612878179694, 5.115463718648684655, 0.01877637416671624343 ) ) ;
#21491 = FACE_OUTER_BOUND ( 'NONE', #9983, .T. ) ;
#21492 = CARTESIAN_POINT ( 'NONE',  ( -0.2819296736111110979, 0.2437499999241333759, -3.452642723725051716E-17 ) ) ;
#21493 = CARTESIAN_POINT ( 'NONE',  ( 0.1993543840281266910, 0.1118055554796889145, -0.1993543840281266910 ) ) ;
#21494 = CARTESIAN_POINT ( 'NONE',  ( -0.3119999999999999996, 0.3236111111111107941, -3.820898013339742174E-17 ) ) ;
#21495 = CARTESIAN_POINT ( 'NONE',  ( 0.3072960869570707798, 4.083864392164723967, 0.05794554327026871926 ) ) ;
#21496 = CARTESIAN_POINT ( 'NONE',  ( 0.2923287055106771337, 0.2723214284738861291, 0.2123892367102621359 ) ) ;
#21497 = CARTESIAN_POINT ( 'NONE',  ( -0.2087850922559471578, 5.050207145506960593, -0.2334572881547273548 ) ) ;
#21498 = DIRECTION ( 'NONE',  ( 0.4999999999999994449, -0.8660254037844390407, 0.000000000000000000 ) ) ;
#21499 = CARTESIAN_POINT ( 'NONE',  ( -0.04066006786217810781, 4.656110604545615317, -0.3119999479932474840 ) ) ;
#21500 = EDGE_LOOP ( 'NONE', ( #9554, #7320, #13709 ) ) ;
#21501 = CARTESIAN_POINT ( 'NONE',  ( -0.2819296736111110979, 3.852861111186976828, 0.000000000000000000 ) ) ;
#21502 = CARTESIAN_POINT ( 'NONE',  ( 0.4687500000000003886, -0.2170120125989245807, 0.07051005015414461841 ) ) ;
#21503 = CARTESIAN_POINT ( 'NONE',  ( 0.05604226080982818020, 5.017622031331995913, 0.3069361942873307658 ) ) ;
#21504 = FACE_OUTER_BOUND ( 'NONE', #19197, .T. ) ;
#21505 = CARTESIAN_POINT ( 'NONE',  ( 0.7463359724041158660, 2.506999999999999673, -2.749000000000000554 ) ) ;
#21506 = CARTESIAN_POINT ( 'NONE',  ( -0.1292346314604056745, 4.491750000151731648, -0.3119999999999999996 ) ) ;
#21507 = CARTESIAN_POINT ( 'NONE',  ( -1.726321361862525858E-17, 4.741750000075866112, -0.2819296736111110979 ) ) ;
#21508 = EDGE_LOOP ( 'NONE', ( #7484, #11618, #20363, #22544 ) ) ;
#21509 = CARTESIAN_POINT ( 'NONE',  ( 0.2819296736111110424, 4.050777777853642903, -0.1167790944451423396 ) ) ;
#21510 = AXIS2_PLACEMENT_3D ( 'NONE', #14491, #21556, #12199 ) ;
#21511 = ADVANCED_FACE ( 'NONE', ( #16790 ), #1073, .F. ) ;
#21512 = ORIENTED_EDGE ( 'NONE', *, *, #7067, .T. ) ;
#21513 = DATE_AND_TIME ( #13851, #8769 ) ;
#21514 = ORIENTED_EDGE ( 'NONE', *, *, #1277, .T. ) ;
#21515 = FACE_OUTER_BOUND ( 'NONE', #14449, .T. ) ;
#21516 = LINE ( 'NONE', #3109, #9276 ) ;
#21517 = CARTESIAN_POINT ( 'NONE',  ( 0.3119999999999999996, 0.01111111095937818323, 0.000000000000000000 ) ) ;
#21518 = CARTESIAN_POINT ( 'NONE',  ( -0.1868639192671823768, 3.514980167629567998, 3.137089416182696766 ) ) ;
#21519 = CARTESIAN_POINT ( 'NONE',  ( -0.4591127969567741496, -0.1126020057588260487, 0.4269506497667299172 ) ) ;
#21520 = CARTESIAN_POINT ( 'NONE',  ( 0.1817294119778012085, 0.2568935841375707407, -0.7276602140724116596 ) ) ;
#21521 = ORIENTED_EDGE ( 'NONE', *, *, #11086, .T. ) ;
#21522 = ORIENTED_EDGE ( 'NONE', *, *, #61, .F. ) ;
#21523 = DIRECTION ( 'NONE',  ( -0.000000000000000000, -1.000000000000000000, -0.000000000000000000 ) ) ;
#21524 = DIRECTION ( 'NONE',  ( 0.000000000000000000, -0.000000000000000000, 1.000000000000000000 ) ) ;
#21525 = CARTESIAN_POINT ( 'NONE',  ( 0.1144950937579609085, -0.2764156081756484751, 0.1056944444444464504 ) ) ;
#21526 = VECTOR ( 'NONE', #3299, 39.37007874015748854 ) ;
#21527 = CARTESIAN_POINT ( 'NONE',  ( -0.1167790944451423535, 4.363277777853642903, 0.2819296736111110424 ) ) ;
#21528 = CARTESIAN_POINT ( 'NONE',  ( 0.3125000000000009437, -0.1294417382415913309, 0.4181944444444486986 ) ) ;
#21529 = ADVANCED_FACE ( 'NONE', ( #10197 ), #22977, .T. ) ;
#21530 = CARTESIAN_POINT ( 'NONE',  ( -1.322549964794167179E-16, 0.7885332705621128646, -1.079944001585411595 ) ) ;
#21531 = LINE ( 'NONE', #1420, #3985 ) ;
#21532 = CARTESIAN_POINT ( 'NONE',  ( 0.3119999999999999996, 0.4555555554038225874, 0.000000000000000000 ) ) ;
#21533 = EDGE_CURVE ( 'NONE', #20507, #5797, #10441, .T. ) ;
#21534 = CARTESIAN_POINT ( 'NONE',  ( -0.3119999999999999996, 4.161888888888888083, 0.000000000000000000 ) ) ;
#21535 = ADVANCED_FACE ( 'NONE', ( #21515 ), #9955, .F. ) ;
#21536 = CARTESIAN_POINT ( 'NONE',  ( -0.1294417382415922191, 0.3125000000000000000, 0.1612500000000022526 ) ) ;
#21537 = CARTESIAN_POINT ( 'NONE',  ( 0.3085230613478114892, 4.973060968630374390, 0.04778564154238736789 ) ) ;
#21538 = CARTESIAN_POINT ( 'NONE',  ( 0.4593750000000003664, 0.2760455974562901482, 0.06112444011295366936 ) ) ;
#21539 = EDGE_LOOP ( 'NONE', ( #6036, #20744, #4489, #20931, #4611, #11473, #5020, #13010 ) ) ;
#21540 = EDGE_CURVE ( 'NONE', #23820, #24032, #21283, .T. ) ;
#21541 = CARTESIAN_POINT ( 'NONE',  ( -0.1907560547815114194, 4.883016371272789868, -0.2468929990473206493 ) ) ;
#21542 = AXIS2_PLACEMENT_3D ( 'NONE', #3615, #11189, #9354 ) ;
#21543 = CARTESIAN_POINT ( 'NONE',  ( 0.4687500000000003886, -0.2630309001378767775, 0.05971062996525598743 ) ) ;
#21544 = CARTESIAN_POINT ( 'NONE',  ( 0.2230971623002953874, -0.2230971623002954429, 0.03104166666666828903 ) ) ;
#21545 = CARTESIAN_POINT ( 'NONE',  ( 0.4450000000000002842, 2.740039370078740433, -2.591000000000000192 ) ) ;
#21546 = CARTESIAN_POINT ( 'NONE',  ( 0.1917387269100320757, 3.815884185560293851, -0.2494959453317835418 ) ) ;
#21547 = CARTESIAN_POINT ( 'NONE',  ( -6.979263641208234666E-17, 0.1187499999024575897, 0.3799334167787516425 ) ) ;
#21548 = DIRECTION ( 'NONE',  ( -0.000000000000000000, -1.000000000000000000, -0.000000000000000000 ) ) ;
#21549 = CARTESIAN_POINT ( 'NONE',  ( 0.1954553509668046640, -0.1954553509668047195, -0.05055555555555479863 ) ) ;
#21550 = CARTESIAN_POINT ( 'NONE',  ( 1.573500000000000343, 0.02500000000000021302, -0.3524999999999999800 ) ) ;
#21551 = DIRECTION ( 'NONE',  ( 0.000000000000000000, 0.000000000000000000, 1.000000000000000000 ) ) ;
#21552 = CARTESIAN_POINT ( 'NONE',  ( -0.2764156081756484196, 1.692557448933383907E-17, 0.4286111111111156613 ) ) ;
#21553 = ORIENTED_EDGE ( 'NONE', *, *, #15758, .F. ) ;
#21554 = CYLINDRICAL_SURFACE ( 'NONE', #11878, 0.3119999999999999996 ) ;
#21555 = CARTESIAN_POINT ( 'NONE',  ( 0.3999999999999999667, 0.1178571428571428131, -0.1299678784931625197 ) ) ;
#21556 = DIRECTION ( 'NONE',  ( -0.4995222938423280468, -0.04370253788966921987, 0.8651979924482607887 ) ) ;
#21557 = CARTESIAN_POINT ( 'NONE',  ( -0.1292346314604058410, 0.4451388888888885287, 0.3119999999999998885 ) ) ;
#21558 = CARTESIAN_POINT ( 'NONE',  ( 0.2206173157302028787, 4.960499999999998799, 0.2206173157302027954 ) ) ;
#21559 = CARTESIAN_POINT ( 'NONE',  ( 0.1993543840281266633, 4.165361111186975940, -0.1993543840281266910 ) ) ;
#21560 = AXIS2_PLACEMENT_3D ( 'NONE', #16137, #9660, #14914 ) ;
#21561 = CARTESIAN_POINT ( 'NONE',  ( 0.1993543840281266633, 4.012583333409199149, -0.1993543840281266910 ) ) ;
#21562 = CARTESIAN_POINT ( 'NONE',  ( 5.731347020009612645E-17, 4.620222222222221120, 0.3119999999999999996 ) ) ;
#21563 = CARTESIAN_POINT ( 'NONE',  ( -0.1517119284478178620, 0.4426845032613772601, 0.4305326508994914980 ) ) ;
#21564 = CARTESIAN_POINT ( 'NONE',  ( 0.3108819030004250084, 4.807000738355847069, 0.02639019689791599274 ) ) ;
#21565 = DIRECTION ( 'NONE',  ( -0.000000000000000000, -1.000000000000000000, -0.000000000000000000 ) ) ;
#21566 = CARTESIAN_POINT ( 'NONE',  ( 0.1167790944451424368, 4.592444444520309865, 0.2819296736111110424 ) ) ;
#21567 = CARTESIAN_POINT ( 'NONE',  ( 0.1116596296178199860, 0.008035714188171883682, -0.3436530038418508792 ) ) ;
#21568 = CARTESIAN_POINT ( 'NONE',  ( 0.1292346314604080892, 3.811194444444443885, -0.3119999999999975016 ) ) ;
#21569 = APPLICATION_PROTOCOL_DEFINITION ( 'international standard', 'config_control_design', 1994, #6704 ) ;
#21570 = DIRECTION ( 'NONE',  ( -0.000000000000000000, 1.000000000000000000, -0.000000000000000000 ) ) ;
#21571 = CARTESIAN_POINT ( 'NONE',  ( 0.1144950937579609085, -0.2764156081756484751, -0.06097222222222153931 ) ) ;
#21572 = CARTESIAN_POINT ( 'NONE',  ( 0.1167790944451422702, 4.127166666742532186, -0.2819296736111110979 ) ) ;
#21573 = VECTOR ( 'NONE', #18062, 39.37007874015748854 ) ;
#21574 = CARTESIAN_POINT ( 'NONE',  ( -0.03977763657374241979, 4.822768489001279413, -0.3096144168800403773 ) ) ;
#21575 = FACE_OUTER_BOUND ( 'NONE', #4439, .T. ) ;
#21576 = CARTESIAN_POINT ( 'NONE',  ( -0.2764156081756484196, 0.1144950937579609918, 0.1473611111111134409 ) ) ;
#21577 = CARTESIAN_POINT ( 'NONE',  ( -0.1116596296178200276, -0.009821428668970967266, 0.3436530038418508792 ) ) ;
#21578 = CARTESIAN_POINT ( 'NONE',  ( 0.1167790944451423257, 0.1013888888130222432, -0.2819296736111110424 ) ) ;
#21579 = CARTESIAN_POINT ( 'NONE',  ( -0.2816345655934842651, 0.09282869753838723925, 0.4076009914526265154 ) ) ;
#21580 = CARTESIAN_POINT ( 'NONE',  ( -0.3120000000000000551, 0.1048611111111107663, 0.1292346314604056190 ) ) ;
#21581 = LINE ( 'NONE', #17572, #6240 ) ;
#21582 = CARTESIAN_POINT ( 'NONE',  ( 0.2764156081756484196, -5.077672346800151106E-17, 0.005000000000001210074 ) ) ;
#21583 = CARTESIAN_POINT ( 'NONE',  ( 0.3155070326520292290, 0.1306872919485615736, 0.3157638888888923967 ) ) ;
#21584 = ORIENTED_EDGE ( 'NONE', *, *, #11057, .F. ) ;
#21585 = EDGE_LOOP ( 'NONE', ( #13729, #16993, #8517, #3632 ) ) ;
#21586 = CARTESIAN_POINT ( 'NONE',  ( 0.000000000000000000, 0.1199999999999999956, 0.000000000000000000 ) ) ;
#21587 = CARTESIAN_POINT ( 'NONE',  ( -0.4581189881604794678, -0.2644951211353319120, 0.3941886329748524598 ) ) ;
#21588 =( BOUNDED_CURVE ( )  B_SPLINE_CURVE ( 2, ( #21064, #11809, #15580, #19356, #23002, #3369, #10820, #14228, #10581 ),
 .UNSPECIFIED., .F., .F. ) 
 B_SPLINE_CURVE_WITH_KNOTS ( ( 3, 2, 2, 2, 3 ),
 ( 0.4791666666666667407, 0.4895833333333333703, 0.5000000000000001110, 0.5104166666666667407, 0.5208333333333334814 ),
 .UNSPECIFIED. ) 
 CURVE ( )  GEOMETRIC_REPRESENTATION_ITEM ( )  RATIONAL_B_SPLINE_CURVE ( ( 0.9999999999999995559, 0.9238795325112871826, 1.000000000000000000, 0.9238795325112867385, 1.000000000000000000, 0.9238795325112867385, 1.000000000000000000, 0.9238795325112859613, 1.000000000000000888 ) ) 
 REPRESENTATION_ITEM ( '' )  );
#21589 = CARTESIAN_POINT ( 'NONE',  ( 0.3248054181707789589, 2.594805418170778921, -0.1201945818292202289 ) ) ;
#21590 = CARTESIAN_POINT ( 'NONE',  ( -0.1167790944451422702, 0.4972222221463556413, -0.2819296736111110424 ) ) ;
#21591 = CARTESIAN_POINT ( 'NONE',  ( 0.2819296736111110979, 4.002166666742532186, 0.1167790944451422425 ) ) ;
#21592 = CARTESIAN_POINT ( 'NONE',  ( 0.3613381517857143232, 0.01517857133102903065, -0.1174058825155740587 ) ) ;
#21593 = ORIENTED_EDGE ( 'NONE', *, *, #8468, .F. ) ;
#21594 = CARTESIAN_POINT ( 'NONE',  ( 0.2819296736111110979, 4.727861111186976828, -3.452642723725051716E-17 ) ) ;
#21595 = CARTESIAN_POINT ( 'NONE',  ( 0.3060896505723387229, 5.131432179253541115, -0.01842300014300301755 ) ) ;
#21596 = CARTESIAN_POINT ( 'NONE',  ( 0.2206173157302027676, 0.3930555554038225874, 0.2206173157302028787 ) ) ;
#21597 = VERTEX_POINT ( 'NONE', #21639 ) ;
#21598 = B_SPLINE_CURVE_WITH_KNOTS ( 'NONE', 3,
 ( #9975, #8613, #8481, #15808, #6300, #17402 ),
 .UNSPECIFIED., .F., .F.,
 ( 4, 2, 4 ),
 ( 0.000000000000000000, 0.0002551367231383052498, 0.0005102734462766104996 ),
 .UNSPECIFIED. ) ;
#21599 = CARTESIAN_POINT ( 'NONE',  ( 0.3125000000000000000, -5.740531871003217465E-17, -0.07833333333333296344 ) ) ;
#21600 = CARTESIAN_POINT ( 'NONE',  ( -0.2819296736111110979, 5.130638888964754507, 0.000000000000000000 ) ) ;
#21601 = VECTOR ( 'NONE', #4690, 39.37007874015748143 ) ;
#21602 = CARTESIAN_POINT ( 'NONE',  ( 0.2730120068861431881, 4.201137816707454675, -0.1516840408520623573 ) ) ;
#21603 = LENGTH_MEASURE_WITH_UNIT ( LENGTH_MEASURE( 0.02539999999999999897 ), #17348 );
#21604 = CARTESIAN_POINT ( 'NONE',  ( 0.1510366717642406820, 0.03242967361111057795, 0.2384937495143246711 ) ) ;
#21605 = APPROVAL_PERSON_ORGANIZATION ( #17320, #23394, #13910 ) ;
#21606 = CARTESIAN_POINT ( 'NONE',  ( 0.1993543840281267465, 4.984805555631420582, 0.1993543840281266633 ) ) ;
#21607 = PERSON_AND_ORGANIZATION ( #15518, #2538 ) ;
#21608 = ORIENTED_EDGE ( 'NONE', *, *, #3070, .T. ) ;
#21609 = DIRECTION ( 'NONE',  ( -0.4999999999999912292, 0.000000000000000000, 0.8660254037844437036 ) ) ;
#21610 = CARTESIAN_POINT ( 'NONE',  ( -5.731347020009612645E-17, 0.2263888888888885564, 0.3119999999999999996 ) ) ;
#21611 = ORIENTED_EDGE ( 'NONE', *, *, #11219, .T. ) ;
#21612 = CARTESIAN_POINT ( 'NONE',  ( -0.1167790944451424368, 0.2541666665908000056, 0.2819296736111110424 ) ) ;
#21613 = ORIENTED_EDGE ( 'NONE', *, *, #20932, .F. ) ;
#21614 = CARTESIAN_POINT ( 'NONE',  ( 0.1167790944451423535, 0.03888888881302225708, 0.2819296736111110424 ) ) ;
#21615 = DIRECTION ( 'NONE',  ( -1.000000000000000000, 0.000000000000000000, 0.000000000000000000 ) ) ;
#21616 = CARTESIAN_POINT ( 'NONE',  ( -0.5116234456863466562, 0.4427737985694510381, 2.549370209580444691 ) ) ;
#21617 = AXIS2_PLACEMENT_3D ( 'NONE', #5104, #12570, #10257 ) ;
#21618 = CARTESIAN_POINT ( 'NONE',  ( 0.1116596296178199027, 0.2651785713310289561, 0.3436530038418508792 ) ) ;
#21619 = CARTESIAN_POINT ( 'NONE',  ( -0.2265706608393805443, 5.064436836433479527, 0.2145077285249635812 ) ) ;
#21620 = DIRECTION ( 'NONE',  ( -1.000000000000000000, -1.224646799147357891E-16, 0.000000000000000000 ) ) ;
#21621 = CARTESIAN_POINT ( 'NONE',  ( 0.2730879860166530726, 3.066692553488282957, 2.936183489075822717 ) ) ;
#21622 = CARTESIAN_POINT ( 'NONE',  ( 0.1993543840281267465, 4.832027777853643791, 0.1993543840281266633 ) ) ;
#21623 = ORIENTED_EDGE ( 'NONE', *, *, #20086, .T. ) ;
#21624 = CARTESIAN_POINT ( 'NONE',  ( -0.2769159822048601893, -0.3938884537237697381, 0.07441357458167788264 ) ) ;
#21625 = CARTESIAN_POINT ( 'NONE',  ( 0.2819296736111110979, 3.821611111186975940, 0.1167790944451422425 ) ) ;
#21626 = CARTESIAN_POINT ( 'NONE',  ( -0.2704407926385273275, 0.05463348271415230384, 0.1405181078658110927 ) ) ;
#21627 = CARTESIAN_POINT ( 'NONE',  ( 0.2829377148481755366, 5.033800763418417645, -0.1314924907175452073 ) ) ;
#21628 = APPROVAL_PERSON_ORGANIZATION ( #21282, #3735, #10440 ) ;
#21629 = CARTESIAN_POINT ( 'NONE',  ( 0.2063516445293624157, 0.05509720184852035657, 0.2244782525227043135 ) ) ;
#21630 = CARTESIAN_POINT ( 'NONE',  ( -0.3236067977499790249, 0.2196428569477723025, 0.2351141009169892271 ) ) ;
#21631 = CARTESIAN_POINT ( 'NONE',  ( 0.3119999999999999996, 4.200083333485066461, -0.1292346314604056745 ) ) ;
#21632 = CARTESIAN_POINT ( 'NONE',  ( -0.1167790944451423535, 4.821611111186976828, 0.2819296736111110979 ) ) ;
#21633 = ORIENTED_EDGE ( 'NONE', *, *, #369, .T. ) ;
#21634 = CARTESIAN_POINT ( 'NONE',  ( 0.1167790944451424368, 4.148000000075866112, 0.2819296736111110424 ) ) ;
#21635 = ORIENTED_EDGE ( 'NONE', *, *, #13984, .T. ) ;
#21636 = CIRCLE ( 'NONE', #9987, 0.2041999999999999926 ) ;
#21637 = ORIENTED_EDGE ( 'NONE', *, *, #9929, .F. ) ;
#21638 = APPROVAL_STATUS ( 'not_yet_approved' ) ;
#21639 = CARTESIAN_POINT ( 'NONE',  ( 0.08808798601667688910, 4.111524471938507119, -3.348023836630494632 ) ) ;
#21640 = DIRECTION ( 'NONE',  ( 0.4985709748471496838, 0.07555085810113111588, 0.8635502596144277732 ) ) ;
#21641 = LOCAL_TIME ( 21, 9, 13.00000000000000000, #12599 ) ;
#21642 = EDGE_LOOP ( 'NONE', ( #19541, #21285, #22026, #1886, #24092, #10176, #2641 ) ) ;
#21643 = CARTESIAN_POINT ( 'NONE',  ( 0.3119999999999999996, 0.2923611109593781676, -0.1292346314604056468 ) ) ;
#21644 = CARTESIAN_POINT ( 'NONE',  ( -0.2476358783382842099, 4.385282689055078009, -0.1900661484681659408 ) ) ;
#21645 = EDGE_CURVE ( 'NONE', #9832, #4238, #17740, .T. ) ;
#21646 = CARTESIAN_POINT ( 'NONE',  ( -0.4687500000000195954, -0.04505700071786207517, 0.4280213696812118496 ) ) ;
#21647 = CARTESIAN_POINT ( 'NONE',  ( 0.2089035349127157382, 0.3994243068236463801, -0.7203251050642737185 ) ) ;
#21648 = ORIENTED_EDGE ( 'NONE', *, *, #7956, .T. ) ;
#21649 = VECTOR ( 'NONE', #4864, 39.37007874015748143 ) ;
#21650 = ORIENTED_EDGE ( 'NONE', *, *, #13522, .T. ) ;
#21651 = CARTESIAN_POINT ( 'NONE',  ( 0.000000000000000000, 5.384999999999999787, -0.3119999999999999996 ) ) ;
#21652 = CARTESIAN_POINT ( 'NONE',  ( -0.1993543840281266633, 0.05624999992413336897, -0.1993543840281266910 ) ) ;
#21653 = CARTESIAN_POINT ( 'NONE',  ( -0.2764156081756484196, -0.1144950937579609362, 0.03625000000000147549 ) ) ;
#21654 = ADVANCED_FACE ( 'NONE', ( #19686 ), #6281, .F. ) ;
#21655 = CARTESIAN_POINT ( 'NONE',  ( -1.726321361862525858E-17, 4.450083333409198261, -0.2819296736111110979 ) ) ;
#21656 = CARTESIAN_POINT ( 'NONE',  ( 0.1514593411830787995, 0.2498004213170063048, -0.08114360514506319122 ) ) ;
#21657 = CARTESIAN_POINT ( 'NONE',  ( -0.2154970682147052952, 0.7011027796760176400, -1.082144637830705358 ) ) ;
#21658 = CYLINDRICAL_SURFACE ( 'NONE', #697, 0.3119999999999999996 ) ;
#21659 = CARTESIAN_POINT ( 'NONE',  ( 0.3119999999999999996, 4.130638888888888971, 0.1292346314604056190 ) ) ;
#21660 = CARTESIAN_POINT ( 'NONE',  ( -0.2206173157302028232, 5.217444444596177178, -0.2206173157302028232 ) ) ;
#21661 = CARTESIAN_POINT ( 'NONE',  ( 0.06250759245605955194, 4.962249824674097809, 0.3056744829715940526 ) ) ;
#21662 = LOCAL_TIME ( 21, 9, 13.00000000000000000, #255 ) ;
#21663 = CARTESIAN_POINT ( 'NONE',  ( 0.000000000000000000, 0.1199999999999999956, 0.000000000000000000 ) ) ;
#21664 = ORIENTED_EDGE ( 'NONE', *, *, #15243, .T. ) ;
#21665 = CARTESIAN_POINT ( 'NONE',  ( 2.310583317527613811, 2.687712728237018567, -2.461238514389269660 ) ) ;
#21666 = B_SPLINE_CURVE_WITH_KNOTS ( 'NONE', 3,
 ( #11981, #4277, #6347, #17329 ),
 .UNSPECIFIED., .F., .F.,
 ( 4, 4 ),
 ( 0.02048720093474762707, 0.02195606945063139845 ),
 .UNSPECIFIED. ) ;
#21667 = ADVANCED_FACE ( 'NONE', ( #12272 ), #17867, .F. ) ;
#21668 = CARTESIAN_POINT ( 'NONE',  ( 0.3155070326520292845, -5.795770164686806123E-17, 0.03798611111111277472 ) ) ;
#21669 = LINE ( 'NONE', #21545, #11669 ) ;
#21670 = EDGE_CURVE ( 'NONE', #10074, #23426, #19563, .T. ) ;
#21671 = CARTESIAN_POINT ( 'NONE',  ( 0.2726213023189543172, 3.803182761333917750, 0.1571292069147020298 ) ) ;
#21672 = EDGE_LOOP ( 'NONE', ( #21735, #16950, #5201, #2999, #20780, #20204 ) ) ;
#21673 = CARTESIAN_POINT ( 'NONE',  ( 2.326421213736078119E-17, 0.1544642856167433020, -0.3799334167787516425 ) ) ;
#21674 = CARTESIAN_POINT ( 'NONE',  ( 1.726321361862525858E-17, 0.1187499999241333620, -0.2819296736111110979 ) ) ;
#21675 = CARTESIAN_POINT ( 'NONE',  ( -0.1954553509668046640, 0.1954553509668046918, -0.02277777777777679341 ) ) ;
#21676 = CARTESIAN_POINT ( 'NONE',  ( 0.2742360776605723416, -0.1498359893662102316, 0.4241666666666772390 ) ) ;
#21677 = DIRECTION ( 'NONE',  ( 0.000000000000000000, 0.7071067811865426878, 0.7071067811865523467 ) ) ;
#21678 = CARTESIAN_POINT ( 'NONE',  ( 3.061616997868383634E-17, 5.580000000000000959, 0.2500000000000000555 ) ) ;
#21679 = ADVANCED_FACE ( 'NONE', ( #4450 ), #19448, .T. ) ;
#21680 = ORIENTED_EDGE ( 'NONE', *, *, #89, .T. ) ;
#21681 = CARTESIAN_POINT ( 'NONE',  ( -0.1913234629623414007, 4.605258746665392700, -0.2464539925195264325 ) ) ;
#21682 = CARTESIAN_POINT ( 'NONE',  ( -0.09533899702212705884, 4.291089024194236323, 0.2976594037573775942 ) ) ;
#21683 = DIRECTION ( 'NONE',  ( -0.000000000000000000, -1.000000000000000000, -0.000000000000000000 ) ) ;
#21684 = CARTESIAN_POINT ( 'NONE',  ( 0.3119999999999999996, 0.4624999999999996336, 0.000000000000000000 ) ) ;
#21685 = CARTESIAN_POINT ( 'NONE',  ( -0.3119999999999999996, 4.828555555555555046, 0.000000000000000000 ) ) ;
#21686 = CARTESIAN_POINT ( 'NONE',  ( -0.1167790944451423119, 4.231333333409199149, -0.2819296736111110979 ) ) ;
#21687 = CARTESIAN_POINT ( 'NONE',  ( 0.1993543840281266633, 3.790361111186977272, -0.1993543840281266910 ) ) ;
#21688 = DIRECTION ( 'NONE',  ( 0.4999999999999912292, 0.000000000000000000, -0.8660254037844437036 ) ) ;
#21689 = FACE_OUTER_BOUND ( 'NONE', #23935, .T. ) ;
#21690 = ORIENTED_EDGE ( 'NONE', *, *, #6726, .T. ) ;
#21691 = CARTESIAN_POINT ( 'NONE',  ( 4.375590819076689459E-17, 0.01607142837634377430, 0.4000000000000000222 ) ) ;
#21692 = CARTESIAN_POINT ( 'NONE',  ( 0.2819296736111110979, 4.602861111186975940, -3.452642723725051716E-17 ) ) ;
#21693 = CYLINDRICAL_SURFACE ( 'NONE', #2978, 0.3125000000000000000 ) ;
#21694 = CARTESIAN_POINT ( 'NONE',  ( 0.4687500000000002776, -0.2598076211353317344, 0.06112444011295376650 ) ) ;
#21695 = DATE_AND_TIME ( #22383, #4856 ) ;
#21696 = DIRECTION ( 'NONE',  ( -0.000000000000000000, -1.000000000000000000, -0.000000000000000000 ) ) ;
#21697 = EDGE_CURVE ( 'NONE', #848, #12392, #2075, .T. ) ;
#21698 = CARTESIAN_POINT ( 'NONE',  ( 0.1144950937579611444, 0.2764156081756483641, 0.07097222222222394905 ) ) ;
#21699 = EDGE_CURVE ( 'NONE', #14885, #20593, #10799, .T. ) ;
#21700 = VECTOR ( 'NONE', #16072, 39.37007874015748143 ) ;
#21701 = CARTESIAN_POINT ( 'NONE',  ( 0.2819296736111111534, 4.113277777853643791, 0.1167790944451422563 ) ) ;
#21702 = CARTESIAN_POINT ( 'NONE',  ( -0.3112736230039412910, 4.834918082158893959, -0.02136994806237297803 ) ) ;
#21703 = CARTESIAN_POINT ( 'NONE',  ( -0.1292346314604088386, 4.894527777777777366, 0.3119999999999968909 ) ) ;
#21704 = CARTESIAN_POINT ( 'NONE',  ( 0.2764156081756484196, -5.077672346800151106E-17, 0.2897222222222257115 ) ) ;
#21705 = CARTESIAN_POINT ( 'NONE',  ( -0.3613381517857143232, 0.1187499999024575897, -4.425116109941954795E-17 ) ) ;
#21706 = CARTESIAN_POINT ( 'NONE',  ( -0.2819296736111110424, 0.004166666590800034188, -0.1167790944451423396 ) ) ;
#21707 = CARTESIAN_POINT ( 'NONE',  ( 0.2209708691207961651, 0.2209708691207959985, -0.06444444444444361042 ) ) ;
#21708 = CARTESIAN_POINT ( 'NONE',  ( -0.3119999999999999996, 0.09791666666666633267, -0.1292346314604056745 ) ) ;
#21709 = FACE_OUTER_BOUND ( 'NONE', #3173, .T. ) ;
#21710 = CARTESIAN_POINT ( 'NONE',  ( -0.2764156081756484196, 0.1144950937579609918, 0.02930555555555695163 ) ) ;
#21711 = CARTESIAN_POINT ( 'NONE',  ( -0.3155070326520293400, 0.1306872919485614903, 0.3365972222222259336 ) ) ;
#21712 = EDGE_CURVE ( 'NONE', #7667, #14283, #24060, .T. ) ;
#21713 = VERTEX_POINT ( 'NONE', #21878 ) ;
#21714 = EDGE_LOOP ( 'NONE', ( #16934, #12646, #17593, #14500 ) ) ;
#21715 = CARTESIAN_POINT ( 'NONE',  ( 0.4253970711649990855, 0.3089455473570085764, 0.05347937985141010958 ) ) ;
#21716 = CARTESIAN_POINT ( 'NONE',  ( 0.4581189881604794123, 0.2644951211353319676, 0.3941886329748524598 ) ) ;
#21717 = CARTESIAN_POINT ( 'NONE',  ( 0.1167790944451423535, 0.4138888888130222155, 0.2819296736111110424 ) ) ;
#21718 = CARTESIAN_POINT ( 'NONE',  ( 0.2819296736111110979, 3.838972222298087544, -3.452642723725051716E-17 ) ) ;
#21719 = CARTESIAN_POINT ( 'NONE',  ( -0.3613381517857143232, -0.02410714295468524213, -4.425116109941954795E-17 ) ) ;
#21720 = ORIENTED_EDGE ( 'NONE', *, *, #239, .T. ) ;
#21721 = CARTESIAN_POINT ( 'NONE',  ( 0.1167790944451422702, 4.571611111186976828, -0.2819296736111110424 ) ) ;
#21722 = CARTESIAN_POINT ( 'NONE',  ( -0.5116234456863466562, 3.066692553488282957, 2.910369331946250249 ) ) ;
#21723 = CARTESIAN_POINT ( 'NONE',  ( -1.910449006669871087E-17, 4.370222222222221120, -0.3119999999999999996 ) ) ;
#21724 = VERTEX_POINT ( 'NONE', #3464 ) ;
#21725 = AXIS2_PLACEMENT_3D ( 'NONE', #21832, #8665, #19647 ) ;
#21726 = CARTESIAN_POINT ( 'NONE',  ( 0.3120000000000000551, 4.019527777777777366, 0.1292346314604056190 ) ) ;
#21727 = CARTESIAN_POINT ( 'NONE',  ( -0.1292346314604057023, 3.734805555707287450, 0.3119999999999998885 ) ) ;
#21728 = CARTESIAN_POINT ( 'NONE',  ( 0.2329872879727148405, 4.203065777311293161, -0.2075117620790080109 ) ) ;
#21729 = LENGTH_MEASURE_WITH_UNIT ( LENGTH_MEASURE( 0.02539999999999999897 ), #14293 );
#21730 = CARTESIAN_POINT ( 'NONE',  ( -0.2819296736111110979, 4.963972222298087544, 0.000000000000000000 ) ) ;
#21731 = ITEM_DEFINED_TRANSFORMATION ( 'NONE', 'NONE', #10310,  #9127 ) ;
#21732 = EDGE_LOOP ( 'NONE', ( #14850, #13123, #10722, #3719, #21720, #21633, #18587, #23323 ) ) ;
#21733 = PLANE ( 'NONE',  #12514 ) ;
#21734 = CARTESIAN_POINT ( 'NONE',  ( -0.2594808896536389686, 4.563054605363555893, 0.1777663154329622852 ) ) ;
#21735 = ORIENTED_EDGE ( 'NONE', *, *, #6776, .T. ) ;
#21736 = CARTESIAN_POINT ( 'NONE',  ( 0.1167790944451423535, 0.3166666665908000056, 0.2819296736111110424 ) ) ;
#21737 = CIRCLE ( 'NONE', #1493, 0.01874999999999997155 ) ;
#21738 = CARTESIAN_POINT ( 'NONE',  ( -0.2819296736111110424, 0.07361111103524449473, -0.1167790944451423396 ) ) ;
#21739 = CARTESIAN_POINT ( 'NONE',  ( -0.2284438653877429726, 4.731022001090376072, 0.2152624247096975307 ) ) ;
#21740 = CARTESIAN_POINT ( 'NONE',  ( -0.1669986196823105007, 5.194782195289050719, -0.2341252263734615313 ) ) ;
#21741 = CARTESIAN_POINT ( 'NONE',  ( -0.2923287055106771337, 0.3937499999024575148, 0.2123892367102619971 ) ) ;
#21742 = CARTESIAN_POINT ( 'NONE',  ( -0.07645976968530923679, 5.045943673328737056, -0.3031838258476152181 ) ) ;
#21743 = EDGE_CURVE ( 'NONE', #10268, #431, #16521, .T. ) ;
#21744 = CARTESIAN_POINT ( 'NONE',  ( -2.307748244742446386E-07, 4.182713274783838919, 0.3119999999998222528 ) ) ;
#21745 = DIRECTION ( 'NONE',  ( 0.4985709748471496838, 0.07555085810113111588, -0.8635502596144277732 ) ) ;
#21746 = CARTESIAN_POINT ( 'NONE',  ( -0.2819296736111110424, 4.752166666742533074, -0.1167790944451423119 ) ) ;
#21747 = CARTESIAN_POINT ( 'NONE',  ( 0.1457644982981150250, 4.520328994860446592, 0.2772101093080964196 ) ) ;
#21748 = CARTESIAN_POINT ( 'NONE',  ( 0.1993543840281266633, 5.234805555631421470, -0.1993543840281266910 ) ) ;
#21749 = CARTESIAN_POINT ( 'NONE',  ( 0.4687500000000002776, 0.2170121405309677343, 0.07051002209705400925 ) ) ;
#21750 = DIRECTION ( 'NONE',  ( 1.000000000000000000, 0.000000000000000000, 0.000000000000000000 ) ) ;
#21751 = CARTESIAN_POINT ( 'NONE',  ( -0.4593750000000003664, -0.2760455974562900927, 0.06112444011295366242 ) ) ;
#21752 = DIRECTION ( 'NONE',  ( -1.000000000000000000, -1.224646799147353700E-16, 0.000000000000000000 ) ) ;
#21753 = CARTESIAN_POINT ( 'NONE',  ( 0.2206173157302028787, 4.356333333485065573, 0.2206173157302027954 ) ) ;
#21754 = CARTESIAN_POINT ( 'NONE',  ( 0.2819296736111111534, 4.779944444520310753, 0.1167790944451422563 ) ) ;
#21755 = CARTESIAN_POINT ( 'NONE',  ( 0.2819296736111110979, 3.769527777853642903, -3.452642723725051716E-17 ) ) ;
#21756 = VECTOR ( 'NONE', #13091, 39.37007874015748143 ) ;
#21757 = ORIENTED_EDGE ( 'NONE', *, *, #7836, .F. ) ;
#21758 =( BOUNDED_CURVE ( )  B_SPLINE_CURVE ( 2, ( #1773, #24079, #1297, #22256, #20193, #3482, #23708, #22014, #14471 ),
 .UNSPECIFIED., .F., .T. ) 
 B_SPLINE_CURVE_WITH_KNOTS ( ( 3, 2, 2, 2, 3 ),
 ( 0.5208333333333333703, 0.5312500000000000000, 0.5416666666666666297, 0.5520833333333333703, 0.5625000000000000000 ),
 .UNSPECIFIED. ) 
 CURVE ( )  GEOMETRIC_REPRESENTATION_ITEM ( )  RATIONAL_B_SPLINE_CURVE ( ( 1.000000000000000000, 0.9238795325112867385, 1.000000000000000000, 0.9238795325112867385, 1.000000000000000000, 0.9238795325112867385, 1.000000000000000000, 0.9238795325112867385, 1.000000000000000000 ) ) 
 REPRESENTATION_ITEM ( '' )  );
#21759 = SHAPE_DEFINITION_REPRESENTATION ( #23527, #17931 ) ;
#21760 = CC_DESIGN_DATE_AND_TIME_ASSIGNMENT ( #1280, #16035, ( #8791 ) ) ;
#21761 = CARTESIAN_POINT ( 'NONE',  ( 2.986000000000000210, 0.05000000000000028727, -2.541000000000000369 ) ) ;
#21762 = CARTESIAN_POINT ( 'NONE',  ( 0.9384745360904206413, 2.661358883302036293, -1.341513222734410871 ) ) ;
#21763 = ORIENTED_EDGE ( 'NONE', *, *, #5188, .T. ) ;
#21764 = CARTESIAN_POINT ( 'NONE',  ( 0.1292346314604056745, 0.2437499998482670627, -0.3119999999999999996 ) ) ;
#21765 = CARTESIAN_POINT ( 'NONE',  ( -0.04129347423352384971, 4.378292985746897514, -0.3093854606850361399 ) ) ;
#21766 = DIRECTION ( 'NONE',  ( 0.000000000000000000, 0.000000000000000000, -1.000000000000000000 ) ) ;
#21767 = CARTESIAN_POINT ( 'NONE',  ( -0.06335377612981457629, 0.3803123470876124679, 0.3999999999999999667 ) ) ;
#21768 = ORIENTED_EDGE ( 'NONE', *, *, #20901, .T. ) ;
#21769 = CARTESIAN_POINT ( 'NONE',  ( 0.5997114317030027841, 2.291712385858714729, -1.145928253224826276 ) ) ;
#21770 = CARTESIAN_POINT ( 'NONE',  ( 0.2819296736111110424, 0.3652777777019111105, 0.1167790944451424923 ) ) ;
#21771 = CARTESIAN_POINT ( 'NONE',  ( 0.1954553509668046640, -0.1954553509668047195, -0.001944444444443294917 ) ) ;
#21772 = VERTEX_POINT ( 'NONE', #12635 ) ;
#21773 = CARTESIAN_POINT ( 'NONE',  ( 0.2819296736111110979, 4.377166666742532186, 0.1167790944451422425 ) ) ;
#21774 = CARTESIAN_POINT ( 'NONE',  ( 0.3125000000000000000, -5.740531871003217465E-17, 0.4216666666666709085 ) ) ;
#21775 = CARTESIAN_POINT ( 'NONE',  ( 2.357946643670095987, 0.000000000000000000, -2.935999999999999943 ) ) ;
#21776 = DIRECTION ( 'NONE',  ( 0.000000000000000000, 0.000000000000000000, -1.000000000000000000 ) ) ;
#21777 = CARTESIAN_POINT ( 'NONE',  ( -0.3119999999999998885, 4.165361111111110404, 0.1292346314604058410 ) ) ;
#21778 = CARTESIAN_POINT ( 'NONE',  ( 0.2206173157302027954, 4.981333333485065573, -0.2206173157302028232 ) ) ;
#21779 = EDGE_CURVE ( 'NONE', #19216, #22988, #5296, .T. ) ;
#21780 = CARTESIAN_POINT ( 'NONE',  ( -0.1292346314604032043, 4.151472222222222008, -0.3120000000000024420 ) ) ;
#21781 = ORIENTED_EDGE ( 'NONE', *, *, #22272, .T. ) ;
#21782 = CARTESIAN_POINT ( 'NONE',  ( -0.1939026278979700812, 4.883130061274394862, -0.2444469480974038600 ) ) ;
#21783 = AXIS2_PLACEMENT_3D ( 'NONE', #3634, #11083, #18513 ) ;
#21784 = CC_DESIGN_PERSON_AND_ORGANIZATION_ASSIGNMENT ( #13505, #13266, ( #6827 ) ) ;
#21785 = CARTESIAN_POINT ( 'NONE',  ( -0.3155070326520293400, -0.1306872919485614626, 0.2359027777777810142 ) ) ;
#21786 = CARTESIAN_POINT ( 'NONE',  ( 0.2233192592356399164, 0.4294642856167432687, 0.3073725909049500604 ) ) ;
#21787 = CARTESIAN_POINT ( 'NONE',  ( -0.2206173157302028232, 4.432722222222222008, -0.2206173157302028232 ) ) ;
#21788 = CARTESIAN_POINT ( 'NONE',  ( 0.3613381517857143232, 0.2830357141881717498, -0.1174058825155740587 ) ) ;
#21789 = DIRECTION ( 'NONE',  ( -0.000000000000000000, -0.000000000000000000, -1.000000000000000000 ) ) ;
#21790 = CARTESIAN_POINT ( 'NONE',  ( -0.1954553509668046918, -0.1954553509668046640, 0.1022222222222241989 ) ) ;
#21791 = CARTESIAN_POINT ( 'NONE',  ( 5.178964085587577574E-17, 5.158416666742532186, 0.2819296736111110979 ) ) ;
#21792 = CARTESIAN_POINT ( 'NONE',  ( 0.1366576343437972407, 4.484363875748784700, -0.2809856522123292955 ) ) ;
#21793 = VERTEX_POINT ( 'NONE', #16277 ) ;
#21794 =( BOUNDED_CURVE ( )  B_SPLINE_CURVE ( 2, ( #5415, #10557, #12882, #20297, #3582, #17989, #11034, #18464, #9199 ),
 .UNSPECIFIED., .F., .F. ) 
 B_SPLINE_CURVE_WITH_KNOTS ( ( 3, 2, 2, 2, 3 ),
 ( 0.6517857142857143016, 0.6562500000000000000, 0.6607142857142856984, 0.6651785714285713969, 0.6696428571428570953 ),
 .UNSPECIFIED. ) 
 CURVE ( )  GEOMETRIC_REPRESENTATION_ITEM ( )  RATIONAL_B_SPLINE_CURVE ( ( 1.000000000000000000, 0.9238795325112867385, 1.000000000000000000, 0.9238795325112867385, 1.000000000000000000, 0.9238795325112867385, 1.000000000000000000, 0.9238795325112867385, 1.000000000000000000 ) ) 
 REPRESENTATION_ITEM ( '' )  );
#21795 = CYLINDRICAL_SURFACE ( 'NONE', #10303, 0.3119999999999999996 ) ;
#21796 = VECTOR ( 'NONE', #21404, 39.37007874015748143 ) ;
#21797 = FACE_OUTER_BOUND ( 'NONE', #4525, .T. ) ;
#21798 = CARTESIAN_POINT ( 'NONE',  ( 0.3125000000000000000, 3.827021247335477694E-17, 1.326383476483184332 ) ) ;
#21799 = CARTESIAN_POINT ( 'NONE',  ( 1.950750485851146632, 2.384774948516263482, -1.884674727345843515 ) ) ;
#21800 = CARTESIAN_POINT ( 'NONE',  ( 0.3119999999999999996, 4.800777777777776478, -3.820898013339742174E-17 ) ) ;
#21801 = AXIS2_PLACEMENT_3D ( 'NONE', #17337, #22334, #13102 ) ;
#21802 = B_SPLINE_CURVE_WITH_KNOTS ( 'NONE', 3,
 ( #23152, #4632, #12100, #1581 ),
 .UNSPECIFIED., .F., .F.,
 ( 4, 4 ),
 ( 0.09513879656923393546, 0.09617319050982510442 ),
 .UNSPECIFIED. ) ;
#21803 = CARTESIAN_POINT ( 'NONE',  ( -0.1993543840281266355, 3.915361111186976384, 0.1993543840281267465 ) ) ;
#21804 = LINE ( 'NONE', #8750, #15545 ) ;
#21805 = DIRECTION ( 'NONE',  ( -0.000000000000000000, -0.000000000000000000, -1.000000000000000000 ) ) ;
#21806 = CARTESIAN_POINT ( 'NONE',  ( -0.3119999999999998885, 4.554249999999997911, 0.1292346314604058410 ) ) ;
#21807 = CARTESIAN_POINT ( 'NONE',  ( -0.2819296736111110979, 4.575083333409199149, 0.000000000000000000 ) ) ;
#21808 = CARTESIAN_POINT ( 'NONE',  ( -0.2428671054993716272, 4.508197984795457636, 0.1958561003821059909 ) ) ;
#21809 = EDGE_CURVE ( 'NONE', #13618, #19328, #10915, .T. ) ;
#21810 = CALENDAR_DATE ( 2026, 7, 10 ) ;
#21811 = DIRECTION ( 'NONE',  ( 0.000000000000000000, 0.000000000000000000, 1.000000000000000000 ) ) ;
#21812 = VECTOR ( 'NONE', #9752, 39.37007874015748143 ) ;
#21813 = CARTESIAN_POINT ( 'NONE',  ( 0.1144950937579609085, -0.2764156081756484751, -0.005416666666665539281 ) ) ;
#21814 = CARTESIAN_POINT ( 'NONE',  ( 0.2819296736111111534, 4.057722222298088433, 0.1167790944451422563 ) ) ;
#21815 = CARTESIAN_POINT ( 'NONE',  ( 0.009921425828668055391, 5.162181618341242562, -0.2989828796063835337 ) ) ;
#21816 = DIRECTION ( 'NONE',  ( -0.000000000000000000, -1.000000000000000000, -0.000000000000000000 ) ) ;
#21817 = CARTESIAN_POINT ( 'NONE',  ( -0.1116596296178199582, 0.03303571418817188160, -0.3436530038418508792 ) ) ;
#21818 = CARTESIAN_POINT ( 'NONE',  ( -0.2819296736111110424, 0.05972222214635559273, -0.1167790944451423396 ) ) ;
#21819 = CARTESIAN_POINT ( 'NONE',  ( 0.4800180059626117934, 0.1716568225058809349, 0.06108596828699448811 ) ) ;
#21820 = CARTESIAN_POINT ( 'NONE',  ( 0.06335377612981449302, 0.01790193843158826431, 0.4000000000000000222 ) ) ;
#21821 = CARTESIAN_POINT ( 'NONE',  ( 0.000000000000000000, 5.384999999999999787, 0.000000000000000000 ) ) ;
#21822 = CARTESIAN_POINT ( 'NONE',  ( 0.2764156081756483641, -0.1144950937579611028, 0.001527777777778966360 ) ) ;
#21823 = CARTESIAN_POINT ( 'NONE',  ( -0.3155070326520292845, 1.931923388228935888E-17, 0.3956250000000041123 ) ) ;
#21824 = VERTEX_POINT ( 'NONE', #20055 ) ;
#21825 = ORIENTED_EDGE ( 'NONE', *, *, #3851, .T. ) ;
#21826 = CARTESIAN_POINT ( 'NONE',  ( -0.5116234456863468782, 3.514980167629567998, 2.549370209580444246 ) ) ;
#21827 = CARTESIAN_POINT ( 'NONE',  ( 0.1294417382415921358, -0.3125000000000002220, 0.02236111111111226818 ) ) ;
#21828 = CARTESIAN_POINT ( 'NONE',  ( 0.2819296736111110979, 0.5354166665908000056, 0.000000000000000000 ) ) ;
#21829 = CARTESIAN_POINT ( 'NONE',  ( -0.2819296736111110424, 3.759111111186976828, 0.1167790944451424923 ) ) ;
#21830 = CARTESIAN_POINT ( 'NONE',  ( 0.2923287055106771337, 0.004464285616743319737, 0.2123892367102621359 ) ) ;
#21831 = CARTESIAN_POINT ( 'NONE',  ( -0.2819296736111110424, 4.418833333409199149, -0.1167790944451423119 ) ) ;
#21832 = CARTESIAN_POINT ( 'NONE',  ( 0.000000000000000000, 3.738758431839877614E-19, -0.1199999999999999956 ) ) ;
#21833 = ADVANCED_FACE ( 'NONE', ( #1757 ), #5169, .T. ) ;
#21834 = AXIS2_PLACEMENT_3D ( 'NONE', #15121, #7435, #5229 ) ;
#21835 = CARTESIAN_POINT ( 'NONE',  ( -5.731347020009612645E-17, 0.1638888887371559577, 0.3119999999999999996 ) ) ;
#21836 = VECTOR ( 'NONE', #16746, 39.37007874015748854 ) ;
#21837 = ORIENTED_EDGE ( 'NONE', *, *, #10878, .T. ) ;
#21838 = EDGE_CURVE ( 'NONE', #18699, #24096, #3108, .T. ) ;
#21839 = CARTESIAN_POINT ( 'NONE',  ( -0.2800968539712042626, 1.715098578335394762E-17, -0.06926352063787094560 ) ) ;
#21840 = CARTESIAN_POINT ( 'NONE',  ( -0.1993543840281266910, 5.179250000075866112, -0.1993543840281266910 ) ) ;
#21841 = CARTESIAN_POINT ( 'NONE',  ( 0.2181460042443824077, 4.203673976828415704, -0.2235058125270818763 ) ) ;
#21842 = EDGE_CURVE ( 'NONE', #12796, #10917, #21794, .T. ) ;
#21843 =( LENGTH_UNIT ( ) NAMED_UNIT ( * ) SI_UNIT ( $, .METRE. ) );
#21844 = DIRECTION ( 'NONE',  ( 0.000000000000000000, 0.000000000000000000, -1.000000000000000000 ) ) ;
#21845 = CARTESIAN_POINT ( 'NONE',  ( 0.1993543840281266633, 4.943138888964754507, -0.1993543840281266910 ) ) ;
#21846 = ITEM_DEFINED_TRANSFORMATION ( 'NONE', 'NONE', #6002,  #9127 ) ;
#21847 = ORIENTED_EDGE ( 'NONE', *, *, #6670, .F. ) ;
#21848 = DIRECTION ( 'NONE',  ( -1.000000000000000000, 0.000000000000000000, 4.440892098500625176E-16 ) ) ;
#21849 = CARTESIAN_POINT ( 'NONE',  ( 0.000000000000000000, 2.291712385858714729, 0.03922008423644621905 ) ) ;
#21850 = VERTEX_POINT ( 'NONE', #16640 ) ;
#21851 = CARTESIAN_POINT ( 'NONE',  ( -5.178964085587577574E-17, 0.3687499999241333204, 0.2819296736111110979 ) ) ;
#21852 = VECTOR ( 'NONE', #3526, 39.37007874015748143 ) ;
#21853 = CARTESIAN_POINT ( 'NONE',  ( 0.1167790944451423535, 0.09444444436857780956, 0.2819296736111110424 ) ) ;
#21854 = CARTESIAN_POINT ( 'NONE',  ( 2.556721741255282954, 0.000000000000000000, -2.088288568297006265 ) ) ;
#21855 = CARTESIAN_POINT ( 'NONE',  ( -0.05462043248617448610, 5.191653777754733134, -0.2846966416326855986 ) ) ;
#21856 = CARTESIAN_POINT ( 'NONE',  ( -0.1236067977499790416, 0.09285714285714280480, 0.3804226065180614236 ) ) ;
#21857 = CARTESIAN_POINT ( 'NONE',  ( 0.3950000000000000733, 2.665000000000000036, -0.6331572882965880167 ) ) ;
#21858 = EDGE_CURVE ( 'NONE', #409, #18846, #20454, .T. ) ;
#21859 = CARTESIAN_POINT ( 'NONE',  ( 0.05000000000000014849, 2.740000000000000213, -2.078583302491978202 ) ) ;
#21860 = CARTESIAN_POINT ( 'NONE',  ( -0.2573147180782621724, 3.885706225055585161, -0.1764478447289662133 ) ) ;
#21861 = CARTESIAN_POINT ( 'NONE',  ( -0.5116234456863258950, 4.111524471938507119, -3.001780280100677434 ) ) ;
#21862 = CARTESIAN_POINT ( 'NONE',  ( -0.2819296736111110424, 4.418833333409199149, -0.1167790944451423119 ) ) ;
#21863 = PLANE ( 'NONE',  #10882 ) ;
#21864 = CARTESIAN_POINT ( 'NONE',  ( -0.2819296736111110979, 5.144527777853643791, 0.000000000000000000 ) ) ;
#21865 = DIRECTION ( 'NONE',  ( 0.8660254037844434816, 0.000000000000000000, 0.4999999999999916178 ) ) ;
#21866 = CARTESIAN_POINT ( 'NONE',  ( 0.3038219221730117936, 4.916572523495020164, 0.08186873057857177449 ) ) ;
#21867 = CARTESIAN_POINT ( 'NONE',  ( -0.4687499999999988898, -0.2570931668155639338, 0.04874733047934373675 ) ) ;
#21868 = ORIENTED_EDGE ( 'NONE', *, *, #23959, .F. ) ;
#21869 = LINE ( 'NONE', #8587, #16723 ) ;
#21870 = CARTESIAN_POINT ( 'NONE',  ( -0.3119999999999999996, 4.332027777929510215, -0.1292346314604056468 ) ) ;
#21871 = CARTESIAN_POINT ( 'NONE',  ( 0.2819296736111111534, 4.502166666742532186, 0.1167790944451422563 ) ) ;
#21872 = CARTESIAN_POINT ( 'NONE',  ( 0.1993543840281267465, 3.762583333409198705, 0.1993543840281266633 ) ) ;
#21873 = EDGE_CURVE ( 'NONE', #23426, #7279, #19522, .T. ) ;
#21874 = EDGE_CURVE ( 'NONE', #24032, #5136, #11391, .T. ) ;
#21875 = ORIENTED_EDGE ( 'NONE', *, *, #20801, .F. ) ;
#21876 = EDGE_LOOP ( 'NONE', ( #22858, #22006, #16546, #21154, #10309, #14421, #4082, #6364, #15284, #23594, #9954, #10040, #17835, #24009, #1549, #7734, #2679, #5531, #912, #8605, #20945, #5306, #19290, #4236 ) ) ;
#21877 = APPROVAL_STATUS ( 'not_yet_approved' ) ;
#21878 = CARTESIAN_POINT ( 'NONE',  ( 0.000000000000000000, 2.665000000000000036, -2.194053356329904947 ) ) ;
#21879 = LINE ( 'NONE', #16039, #24056 ) ;
#21880 = VERTEX_POINT ( 'NONE', #13237 ) ;
#21881 = CARTESIAN_POINT ( 'NONE',  ( 0.1292346314604057023, 0.1673611109593781676, 0.3119999999999998885 ) ) ;
#21882 = CARTESIAN_POINT ( 'NONE',  ( -0.06786238497518067014, 4.379037417340335914, -0.3050586073130007736 ) ) ;
#21883 = CARTESIAN_POINT ( 'NONE',  ( -0.2921947132138422165, 3.721047735574461335, -0.1187172976513048844 ) ) ;
#21884 = DIRECTION ( 'NONE',  ( 0.000000000000000000, 0.000000000000000000, 1.000000000000000000 ) ) ;
#21885 = CARTESIAN_POINT ( 'NONE',  ( 0.1397624911352057520, 0.5346735903725252648, -0.7369254640284191860 ) ) ;
#21886 = ORIENTED_EDGE ( 'NONE', *, *, #10578, .F. ) ;
#21887 = VERTEX_POINT ( 'NONE', #283 ) ;
#21888 = ORIENTED_EDGE ( 'NONE', *, *, #9760, .F. ) ;
#21889 = CARTESIAN_POINT ( 'NONE',  ( -0.2977100099089716734, 3.700000000000000622, -0.09499999999999995948 ) ) ;
#21890 = CARTESIAN_POINT ( 'NONE',  ( -0.1167790944451424506, 0.1847222221463556413, 0.2819296736111110424 ) ) ;
#21891 = CARTESIAN_POINT ( 'NONE',  ( 0.1144950937579609085, -0.2764156081756484751, 0.3834722222222265442 ) ) ;
#21892 = CARTESIAN_POINT ( 'NONE',  ( -0.2819296736111110979, 4.463972222298087544, 0.000000000000000000 ) ) ;
#21893 = CARTESIAN_POINT ( 'NONE',  ( 0.08187103065728440487, 0.2793464338139753922, -0.07965142539470895788 ) ) ;
#21894 = CARTESIAN_POINT ( 'NONE',  ( -0.4687500000000003886, -0.2598076211353319009, 0.06112444011295369711 ) ) ;
#21895 = CARTESIAN_POINT ( 'NONE',  ( -0.04062695888593492732, 4.237158410735314185, 0.3093461996519432100 ) ) ;
#21896 = CARTESIAN_POINT ( 'NONE',  ( -0.3119999999999998885, 4.054249999999998799, 0.1292346314604058410 ) ) ;
#21897 = CARTESIAN_POINT ( 'NONE',  ( 5.731347020009612645E-17, 5.071611111262843252, 0.3119999999999999996 ) ) ;
#21898 = AXIS2_PLACEMENT_3D ( 'NONE', #16442, #18749, #20578 ) ;
#21899 = CARTESIAN_POINT ( 'NONE',  ( -0.5116234456863258950, 4.559812086079793048, -3.041000364337123507 ) ) ;
#21900 = ORIENTED_EDGE ( 'NONE', *, *, #8462, .T. ) ;
#21901 = EDGE_CURVE ( 'NONE', #13148, #10864, #13475, .T. ) ;
#21902 = CARTESIAN_POINT ( 'NONE',  ( 0.009844691510165828885, 4.682939453713771627, 0.3119999979940254464 ) ) ;
#21903 = CARTESIAN_POINT ( 'NONE',  ( -0.3155070326520293400, 0.1306872919485614903, 0.2845138888888925077 ) ) ;
#21904 = LINE ( 'NONE', #12663, #12440 ) ;
#21905 = CARTESIAN_POINT ( 'NONE',  ( -0.5601250000000235207, -6.859552883724400952E-17, -0.05999999999999999084 ) ) ;
#21906 = CARTESIAN_POINT ( 'NONE',  ( 0.3950000000000000178, 2.665000000000000036, -1.966000000000000192 ) ) ;
#21907 = CARTESIAN_POINT ( 'NONE',  ( -0.1993543840281266633, 0.2368055554796889006, -0.1993543840281266910 ) ) ;
#21908 = CARTESIAN_POINT ( 'NONE',  ( 0.000000000000000000, 0.2764156081756484196, 0.3036111111111146621 ) ) ;
#21909 = EDGE_CURVE ( 'NONE', #2426, #14570, #5888, .T. ) ;
#21910 = CARTESIAN_POINT ( 'NONE',  ( -0.2819296736111110424, 5.196611111186976828, -0.1167790944451423119 ) ) ;
#21911 = CARTESIAN_POINT ( 'NONE',  ( 0.3040713822389952137, 4.472421292987645458, 0.06995111167926036655 ) ) ;
#21912 = CARTESIAN_POINT ( 'NONE',  ( 0.000000000000000000, 5.384999999999999787, 0.000000000000000000 ) ) ;
#21913 = CARTESIAN_POINT ( 'NONE',  ( 0.02885018458022743301, 4.876384086389262684, -0.3107525876215130878 ) ) ;
#21914 = CARTESIAN_POINT ( 'NONE',  ( 0.000000000000000000, 6.000000000000000888, -0.3125000000000000555 ) ) ;
#21915 = CARTESIAN_POINT ( 'NONE',  ( -0.4784936136544858387, 0.2687202946394925962, 0.04212966708837331820 ) ) ;
#21916 = CARTESIAN_POINT ( 'NONE',  ( 0.3119999999999999996, 4.693138888888888971, -0.1292346314604056745 ) ) ;
#21917 = B_SPLINE_CURVE_WITH_KNOTS ( 'NONE', 3,
 ( #15455, #692, #11796, #8237, #6297, #21295, #23105, #17280 ),
 .UNSPECIFIED., .F., .F.,
 ( 4, 2, 2, 4 ),
 ( 8.673617379884035472E-19, 0.001711848256466968511, 0.003423696512933936155, 0.006847393025867874912 ),
 .UNSPECIFIED. ) ;
#21918 = CC_DESIGN_DATE_AND_TIME_ASSIGNMENT ( #4179, #2365, ( #2926 ) ) ;
#21919 = CARTESIAN_POINT ( 'NONE',  ( -0.2819296736111110979, 3.908416666742532630, 0.000000000000000000 ) ) ;
#21920 = CARTESIAN_POINT ( 'NONE',  ( -0.2819296736111110424, 3.807722222298089321, -0.1167790944451423119 ) ) ;
#21921 = CARTESIAN_POINT ( 'NONE',  ( -0.3999999999999999667, 0.2178571428571427493, -0.1299678784931626030 ) ) ;
#21922 = FACE_OUTER_BOUND ( 'NONE', #2523, .T. ) ;
#21923 = PLANE ( 'NONE',  #15181 ) ;
#21924 = CARTESIAN_POINT ( 'NONE',  ( -0.2819296736111110979, 4.463972222298087544, 0.000000000000000000 ) ) ;
#21925 = AXIS2_PLACEMENT_3D ( 'NONE', #7520, #22391, #5692 ) ;
#21926 = CARTESIAN_POINT ( 'NONE',  ( 0.3119999999999999996, 0.07361111111111078020, 0.000000000000000000 ) ) ;
#21927 = CARTESIAN_POINT ( 'NONE',  ( -0.1144950937579609779, 0.2764156081756484196, 0.1334722222222244348 ) ) ;
#21928 = CARTESIAN_POINT ( 'NONE',  ( 0.1167790944451422702, 3.849388888964754951, -0.2819296736111110979 ) ) ;
#21929 = CARTESIAN_POINT ( 'NONE',  ( 0.000000000000000000, 0.000000000000000000, 1.326383476483184332 ) ) ;
#21930 = CARTESIAN_POINT ( 'NONE',  ( 0.09770977851924383950, 5.159011269489411688, -0.2842526675492763055 ) ) ;
#21931 =( BOUNDED_CURVE ( )  B_SPLINE_CURVE ( 2, ( #17641, #21418, #14106, #10216, #12292 ),
 .UNSPECIFIED., .F., .T. ) 
 B_SPLINE_CURVE_WITH_KNOTS ( ( 3, 2, 3 ),
 ( 0.1285401400649176518, 0.1294642857142857262, 0.1339285714285714246 ),
 .UNSPECIFIED. ) 
 CURVE ( )  GEOMETRIC_REPRESENTATION_ITEM ( )  RATIONAL_B_SPLINE_CURVE ( ( 0.9750087287892017507, 0.9842424066559070095, 1.000000000000000000, 0.9238795325112867385, 1.000000000000000000 ) ) 
 REPRESENTATION_ITEM ( '' )  );
#21932 = DIRECTION ( 'NONE',  ( 0.000000000000000000, 0.000000000000000000, -1.000000000000000000 ) ) ;
#21933 = EDGE_CURVE ( 'NONE', #3702, #6119, #4096, .T. ) ;
#21934 = CARTESIAN_POINT ( 'NONE',  ( 0.2923287055106771337, 0.01874999990245760501, -0.2123892367102620249 ) ) ;
#21935 = CARTESIAN_POINT ( 'NONE',  ( 0.1167790944451423535, 0.3583333332574666907, 0.2819296736111110424 ) ) ;
#21936 = CARTESIAN_POINT ( 'NONE',  ( -0.1829869529092254532, 0.2292256185136192503, 0.4043689316861039940 ) ) ;
#21937 = DIRECTION ( 'NONE',  ( 0.8660254037844434816, 0.000000000000000000, -0.4999999999999916178 ) ) ;
#21938 = EDGE_CURVE ( 'NONE', #6271, #12631, #992, .T. ) ;
#21939 = CARTESIAN_POINT ( 'NONE',  ( -0.1236067977499790416, 0.1642857142857142294, 0.3804226065180614236 ) ) ;
#21940 = CARTESIAN_POINT ( 'NONE',  ( 0.2764156081756483641, -0.1144950937579611028, 0.05708333333333497073 ) ) ;
#21941 = CARTESIAN_POINT ( 'NONE',  ( 0.2764156081756484196, -5.077672346800151106E-17, -0.04361111111111028865 ) ) ;
#21942 = VECTOR ( 'NONE', #23099, 39.37007874015748143 ) ;
#21943 = VERTEX_POINT ( 'NONE', #3948 ) ;
#21944 = ORIENTED_EDGE ( 'NONE', *, *, #16067, .F. ) ;
#21945 = CARTESIAN_POINT ( 'NONE',  ( 0.000000000000000000, 5.384999999999999787, 0.000000000000000000 ) ) ;
#21946 = CARTESIAN_POINT ( 'NONE',  ( -0.2494959280049152961, 3.829773069302058630, -0.1917387442425347033 ) ) ;
#21947 = CARTESIAN_POINT ( 'NONE',  ( 0.3119999999999999996, 0.1291666666666663188, 0.000000000000000000 ) ) ;
#21948 = CARTESIAN_POINT ( 'NONE',  ( -0.1993543840281266910, 3.804250000075865668, -0.1993543840281266910 ) ) ;
#21949 = CARTESIAN_POINT ( 'NONE',  ( 0.1116596296178199860, 0.3116071427596003862, -0.3436530038418508792 ) ) ;
#21950 = ADVANCED_FACE ( 'NONE', ( #10142 ), #407, .F. ) ;
#21951 = CARTESIAN_POINT ( 'NONE',  ( -0.1993543840281266910, 4.415361111186976828, -0.1993543840281266910 ) ) ;
#21952 = CARTESIAN_POINT ( 'NONE',  ( -5.731347020009612645E-17, 0.1083333331816004053, 0.3119999999999999996 ) ) ;
#21953 = FACE_OUTER_BOUND ( 'NONE', #1232, .T. ) ;
#21954 = ORIENTED_EDGE ( 'NONE', *, *, #19928, .F. ) ;
#21955 = CARTESIAN_POINT ( 'NONE',  ( 0.3999999999999999667, 0.3964285714285711859, 0.1299678784931626307 ) ) ;
#21956 = CARTESIAN_POINT ( 'NONE',  ( 5.178964085587577574E-17, 5.144527777853643791, 0.2819296736111110979 ) ) ;
#21957 = CARTESIAN_POINT ( 'NONE',  ( 0.000000000000000000, 0.1799999999999999933, 0.000000000000000000 ) ) ;
#21958 = CIRCLE ( 'NONE', #2533, 0.3125000000000000000 ) ;
#21959 =( CONVERSION_BASED_UNIT ( 'INCH', #9159 ) LENGTH_UNIT ( ) NAMED_UNIT ( #23314 ) );
#21960 = CARTESIAN_POINT ( 'NONE',  ( 0.3236067977499790249, 0.2553571426620580009, -0.2351141009169892826 ) ) ;
#21961 = CYLINDRICAL_SURFACE ( 'NONE', #6794, 0.3119999999999999996 ) ;
#21962 = CARTESIAN_POINT ( 'NONE',  ( -0.2819296736111110424, 4.800777777853643791, 0.1167790944451424923 ) ) ;
#21963 = APPROVAL_ROLE ( '' ) ;
#21964 = CARTESIAN_POINT ( 'NONE',  ( -0.4607728391470959362, 0.2757711312522204139, 0.04763613967037565872 ) ) ;
#21965 = CARTESIAN_POINT ( 'NONE',  ( -0.3119999999999999996, 0.4243055554038226429, -0.1292346314604056745 ) ) ;
#21966 = VERTEX_POINT ( 'NONE', #22605 ) ;
#21967 = CARTESIAN_POINT ( 'NONE',  ( -0.2819296736111110424, 0.2402777777019111938, -0.1167790944451423396 ) ) ;
#21968 = ADVANCED_FACE ( 'NONE', ( #856 ), #13349, .F. ) ;
#21969 = EDGE_CURVE ( 'NONE', #5797, #22655, #9680, .T. ) ;
#21970 = ORIENTED_EDGE ( 'NONE', *, *, #228, .F. ) ;
#21971 = CARTESIAN_POINT ( 'NONE',  ( -0.1993543840281266633, 0.2923611110352444808, -0.1993543840281266910 ) ) ;
#21972 = DIRECTION ( 'NONE',  ( -4.347502568299324428E-16, 0.7071067811865500152, -0.7071067811865451302 ) ) ;
#21973 = CARTESIAN_POINT ( 'NONE',  ( -0.1076999173815676586, 5.193055214671070452, -0.2685177118993510859 ) ) ;
#21974 = CARTESIAN_POINT ( 'NONE',  ( -7.726019084026502927E-17, -0.04642857142857145097, 0.4205848896953069405 ) ) ;
#21975 = CARTESIAN_POINT ( 'NONE',  ( 0.2230971623002953874, -0.2230971623002954429, 0.02756944444444561770 ) ) ;
#21976 = CARTESIAN_POINT ( 'NONE',  ( 2.936000000000000387, 0.02499999999999983832, -2.566000000000001169 ) ) ;
#21977 = CARTESIAN_POINT ( 'NONE',  ( -5.731347020009612645E-17, 0.1083333331816004053, 0.3119999999999999996 ) ) ;
#21978 = CARTESIAN_POINT ( 'NONE',  ( 0.9473029863927551197, 2.405292355953585925, -1.303818980007233064 ) ) ;
#21979 = CARTESIAN_POINT ( 'NONE',  ( 0.2819296736111110979, 4.557722222298087544, 0.1167790944451422425 ) ) ;
#21980 = CARTESIAN_POINT ( 'NONE',  ( 0.2977100099089716734, 3.575000000000000622, -0.09499999999999993172 ) ) ;
#21981 = CARTESIAN_POINT ( 'NONE',  ( 0.3051448587956195890, 4.531920635835558819, -0.06985392631230002980 ) ) ;
#21982 = TOROIDAL_SURFACE ( 'NONE', #4068, 0.6211549996190571798, 0.01874999999999999931 ) ;
#21983 = EDGE_CURVE ( 'NONE', #23019, #3616, #7841, .T. ) ;
#21984 = CARTESIAN_POINT ( 'NONE',  ( 0.2819296736111110979, 5.113277777853642903, 0.1167790944451422425 ) ) ;
#21985 = CARTESIAN_POINT ( 'NONE',  ( 0.4687500000000002776, -0.2598076211353317344, 0.06112444011295376650 ) ) ;
#21986 = CARTESIAN_POINT ( 'NONE',  ( 0.1570546580433174466, 4.909658102729531848, 0.2726611153537367715 ) ) ;
#21987 = CARTESIAN_POINT ( 'NONE',  ( 0.2170440708343631397, 0.05599619865938067903, 0.2154300401225580364 ) ) ;
#21988 = CARTESIAN_POINT ( 'NONE',  ( -0.03984298593500181646, 4.767186640188652902, -0.3119995727676234121 ) ) ;
#21989 = CARTESIAN_POINT ( 'NONE',  ( -0.3119999999999999996, 4.276472222373953969, -0.1292346314604056468 ) ) ;
#21990 = CARTESIAN_POINT ( 'NONE',  ( 0.2819296736111110979, 4.561194444520310753, -3.452642723725051716E-17 ) ) ;
#21991 = CARTESIAN_POINT ( 'NONE',  ( -1.726321361862525858E-17, 3.783416666742532186, -0.2819296736111110979 ) ) ;
#21992 = VERTEX_POINT ( 'NONE', #11637 ) ;
#21993 = EDGE_CURVE ( 'NONE', #10368, #18493, #13455, .T. ) ;
#21994 = ORIENTED_EDGE ( 'NONE', *, *, #12651, .F. ) ;
#21995 = MECHANICAL_CONTEXT ( 'NONE', #2656, 'mechanical' ) ;
#21996 = CARTESIAN_POINT ( 'NONE',  ( -0.2709282478162917118, -0.1304588658952868796, 0.4118983757380794697 ) ) ;
#21997 = CARTESIAN_POINT ( 'NONE',  ( -5.488040394358968970E-07, 4.960478275469978549, 0.3119999999989728212 ) ) ;
#21998 = FACE_OUTER_BOUND ( 'NONE', #8516, .T. ) ;
#21999 = ORIENTED_EDGE ( 'NONE', *, *, #3343, .T. ) ;
#22000 = CARTESIAN_POINT ( 'NONE',  ( -0.3119999999999999996, 0.2020833331816004053, -0.1292346314604056745 ) ) ;
#22001 = CARTESIAN_POINT ( 'NONE',  ( -0.08148921683276161287, 4.402575570918881631, 0.3039149224628344692 ) ) ;
#22002 = CARTESIAN_POINT ( 'NONE',  ( -0.02028168178945650296, 5.129600928296707885, 0.3068236208125575404 ) ) ;
#22003 = DIRECTION ( 'NONE',  ( 0.5000000000000005551, 0.000000000000000000, -0.8660254037844383745 ) ) ;
#22004 = CARTESIAN_POINT ( 'NONE',  ( 0.1851914621056884036, 0.2629614562125153210, -0.7267838718924568564 ) ) ;
#22005 = ORIENTED_EDGE ( 'NONE', *, *, #97, .T. ) ;
#22006 = ORIENTED_EDGE ( 'NONE', *, *, #3179, .T. ) ;
#22007 = SECURITY_CLASSIFICATION ( '', '', #21219 ) ;
#22008 = ORIENTED_EDGE ( 'NONE', *, *, #18374, .T. ) ;
#22009 = CARTESIAN_POINT ( 'NONE',  ( 7.345979252745889464E-17, -0.5196152422706635798, 0.3779506566538943235 ) ) ;
#22010 = CARTESIAN_POINT ( 'NONE',  ( -0.2764156081756484196, 1.692557448933383907E-17, 0.1994444444444472553 ) ) ;
#22011 = CARTESIAN_POINT ( 'NONE',  ( -0.2819296736111110424, 4.300777777853642903, 0.1167790944451424923 ) ) ;
#22012 = CARTESIAN_POINT ( 'NONE',  ( -0.1167790944451423119, 5.009111111186976828, -0.2819296736111110979 ) ) ;
#22013 = DIRECTION ( 'NONE',  ( -0.6121567523560114132, -0.6746457328860028246, 0.4124527192826460964 ) ) ;
#22014 = CARTESIAN_POINT ( 'NONE',  ( -0.1292346314604058410, 0.3826388887371559022, 0.3119999999999998885 ) ) ;
#22015 = CARTESIAN_POINT ( 'NONE',  ( 0.3119999999999999996, 4.078555555555555046, -3.820898013339742174E-17 ) ) ;
#22016 = CARTESIAN_POINT ( 'NONE',  ( -0.3119999999999998885, 4.950083333485066461, 0.1292346314604058410 ) ) ;
#22017 = AXIS2_PLACEMENT_3D ( 'NONE', #17773, #13999, #4956 ) ;
#22018 = CARTESIAN_POINT ( 'NONE',  ( -0.1167790944451423119, 5.078555555631421470, -0.2819296736111110979 ) ) ;
#22019 = PLANE ( 'NONE',  #2730 ) ;
#22020 = ORIENTED_EDGE ( 'NONE', *, *, #18301, .F. ) ;
#22021 = LOCAL_TIME ( 21, 9, 13.00000000000000000, #18225 ) ;
#22022 = CARTESIAN_POINT ( 'NONE',  ( 0.2832806843015959197, 0.03401755210715768502, 0.01622507305669601205 ) ) ;
#22023 = ORIENTED_EDGE ( 'NONE', *, *, #643, .T. ) ;
#22024 = CARTESIAN_POINT ( 'NONE',  ( -0.1306872919485614903, 0.3155070326520293400, 0.3331250000000040012 ) ) ;
#22025 = CARTESIAN_POINT ( 'NONE',  ( -0.3125000000000000000, 1.913510623667739771E-17, 0.01194444444444589179 ) ) ;
#22026 = ORIENTED_EDGE ( 'NONE', *, *, #566, .T. ) ;
#22027 = VECTOR ( 'NONE', #6645, 39.37007874015748143 ) ;
#22028 = CARTESIAN_POINT ( 'NONE',  ( 0.3999999999999999667, 0.04642857142857139546, -0.1299678784931625197 ) ) ;
#22029 = PLANE ( 'NONE',  #21542 ) ;
#22030 = CARTESIAN_POINT ( 'NONE',  ( -0.1993543840281267465, 0.2506944443685777957, 0.1993543840281266633 ) ) ;
#22031 = CARTESIAN_POINT ( 'NONE',  ( -3.385114897866767815E-17, -0.2764156081756484196, 0.3313888888888926743 ) ) ;
#22032 = EDGE_CURVE ( 'NONE', #21850, #7051, #2922, .T. ) ;
#22033 = CARTESIAN_POINT ( 'NONE',  ( 0.000000000000000000, 0.4987679491924311148, 0.000000000000000000 ) ) ;
#22034 = CARTESIAN_POINT ( 'NONE',  ( 0.1228621477648789984, 4.484786867006959277, -0.2870958250574380255 ) ) ;
#22035 = EDGE_CURVE ( 'NONE', #6320, #12233, #12335, .T. ) ;
#22036 = CARTESIAN_POINT ( 'NONE',  ( -0.1993543840281266355, 4.970916666742532186, 0.1993543840281267465 ) ) ;
#22037 = CARTESIAN_POINT ( 'NONE',  ( -0.2726727406394559017, 4.173537243704723565, 0.1570538247964039513 ) ) ;
#22038 = CARTESIAN_POINT ( 'NONE',  ( 0.0002098633495959924473, 4.877161027885005495, -0.3119999340045161440 ) ) ;
#22039 = LOCAL_TIME ( 21, 9, 13.00000000000000000, #22205 ) ;
#22040 = CARTESIAN_POINT ( 'NONE',  ( 0.3119999999999999996, 4.082027777777776478, -0.1292346314604056745 ) ) ;
#22041 = CARTESIAN_POINT ( 'NONE',  ( 0.3119999999999998885, 0.5631944442927114824, 0.1292346314604058410 ) ) ;
#22042 = CARTESIAN_POINT ( 'NONE',  ( 0.3119999999999999996, 4.741749999999998799, 0.1292346314604056190 ) ) ;
#22043 = CARTESIAN_POINT ( 'NONE',  ( -1.726321361862525858E-17, 4.005638888964754507, -0.2819296736111110979 ) ) ;
#22044 = LINE ( 'NONE', #1801, #20981 ) ;
#22045 = CARTESIAN_POINT ( 'NONE',  ( 0.2734898064461412370, 4.034470968406938418, -0.1527495561689310444 ) ) ;
#22046 = CARTESIAN_POINT ( 'NONE',  ( 0.1292346314604057300, 0.5006944442927115935, 0.3119999999999998885 ) ) ;
#22047 = AXIS2_PLACEMENT_3D ( 'NONE', #1212, #11058, #18486 ) ;
#22048 = DIRECTION ( 'NONE',  ( -1.000000000000000000, 0.000000000000000000, 0.000000000000000000 ) ) ;
#22049 = ORIENTED_EDGE ( 'NONE', *, *, #10701, .F. ) ;
#22050 = CARTESIAN_POINT ( 'NONE',  ( 0.2819296736111110979, 4.210500000075865223, 0.1167790944451422425 ) ) ;
#22051 = CARTESIAN_POINT ( 'NONE',  ( -0.2181590239592449132, 4.509281914422427207, 0.2241040346535229100 ) ) ;
#22052 = CARTESIAN_POINT ( 'NONE',  ( -0.1064715942168695945, -0.2552471790383887273, -0.06558227484231508864 ) ) ;
#22053 = CARTESIAN_POINT ( 'NONE',  ( 0.2764156081756484196, -5.077672346800151106E-17, 0.1716666666666692431 ) ) ;
#22054 = LOCAL_TIME ( 21, 9, 13.00000000000000000, #4274 ) ;
#22055 = FACE_OUTER_BOUND ( 'NONE', #18100, .T. ) ;
#22056 = FACE_OUTER_BOUND ( 'NONE', #22632, .T. ) ;
#22057 = CC_DESIGN_PERSON_AND_ORGANIZATION_ASSIGNMENT ( #8465, #8222, ( #5667 ) ) ;
#22058 = CARTESIAN_POINT ( 'NONE',  ( 0.01277271335453323588, -0.5470360373338564175, 0.04287645741408792344 ) ) ;
#22059 = CARTESIAN_POINT ( 'NONE',  ( 0.2923287055106771337, 0.3616071427596004306, 0.2123892367102621359 ) ) ;
#22060 = AXIS2_PLACEMENT_3D ( 'NONE', #17331, #15030, #22455 ) ;
#22061 = CARTESIAN_POINT ( 'NONE',  ( -0.2819296736111110979, 0.2333333332574667185, 0.1167790944451422425 ) ) ;
#22062 = CARTESIAN_POINT ( 'NONE',  ( 0.2494946377407150639, 3.857550799961272592, 0.1917403518701246146 ) ) ;
#22063 = DIRECTION ( 'NONE',  ( 0.000000000000000000, 0.000000000000000000, 1.000000000000000000 ) ) ;
#22064 = FACE_OUTER_BOUND ( 'NONE', #2121, .T. ) ;
#22065 = CARTESIAN_POINT ( 'NONE',  ( -0.2230971623002953874, 0.2230971623002954152, 0.4997916666666716301 ) ) ;
#22066 = ORIENTED_EDGE ( 'NONE', *, *, #12675, .T. ) ;
#22067 = LINE ( 'NONE', #12227, #11853 ) ;
#22068 = CARTESIAN_POINT ( 'NONE',  ( 0.3119999999999999996, 4.356333333333332725, -3.820898013339742174E-17 ) ) ;
#22069 = CARTESIAN_POINT ( 'NONE',  ( -0.2206173157302028787, -0.002777777777778111818, 0.2206173157302027954 ) ) ;
#22070 = CARTESIAN_POINT ( 'NONE',  ( -0.1993543840281266355, 3.818138888964754507, 0.1993543840281267465 ) ) ;
#22071 = CARTESIAN_POINT ( 'NONE',  ( 2.326421213736078119E-17, 0.3151785713310290005, -0.3799334167787516425 ) ) ;
#22072 = ORIENTED_EDGE ( 'NONE', *, *, #9762, .T. ) ;
#22073 = CARTESIAN_POINT ( 'NONE',  ( 0.1993543840281266633, 4.401472222298088433, -0.1993543840281266910 ) ) ;
#22074 = CARTESIAN_POINT ( 'NONE',  ( 0.2730879860166530726, 3.066692553488282957, 2.936183489075822717 ) ) ;
#22075 = LINE ( 'NONE', #3663, #20002 ) ;
#22076 = ORIENTED_EDGE ( 'NONE', *, *, #10580, .T. ) ;
#22077 = CARTESIAN_POINT ( 'NONE',  ( 0.1426520719866612441, 4.373010559984535917, -0.2781209046996724332 ) ) ;
#22078 = CARTESIAN_POINT ( 'NONE',  ( 0.2819296736111110979, 5.102861111186976828, -3.452642723725051716E-17 ) ) ;
#22079 = CARTESIAN_POINT ( 'NONE',  ( 0.2510418245647489388, 4.202275339918530861, -0.1855358740567382703 ) ) ;
#22080 = TOROIDAL_SURFACE ( 'NONE', #4571, 0.3385998376278290256, 0.01874999999999999931 ) ;
#22081 =( BOUNDED_CURVE ( )  B_SPLINE_CURVE ( 2, ( #23468, #15807, #10574, #13988, #10455, #17882, #8612, #6778, #14221 ),
 .UNSPECIFIED., .F., .T. ) 
 B_SPLINE_CURVE_WITH_KNOTS ( ( 3, 2, 2, 2, 3 ),
 ( 0.1041666666666666990, 0.1145833333333333565, 0.1250000000000000278, 0.1354166666666666852, 0.1458333333333333703 ),
 .UNSPECIFIED. ) 
 CURVE ( )  GEOMETRIC_REPRESENTATION_ITEM ( )  RATIONAL_B_SPLINE_CURVE ( ( 0.9999999999999997780, 0.9238795325112869605, 1.000000000000000000, 0.9238795325112867385, 1.000000000000000000, 0.9238795325112867385, 1.000000000000000000, 0.9238795325112865164, 1.000000000000000222 ) ) 
 REPRESENTATION_ITEM ( '' )  );
#22082 = CARTESIAN_POINT ( 'NONE',  ( 0.000000000000000000, 5.384999999999999787, 0.000000000000000000 ) ) ;
#22083 = DIRECTION ( 'NONE',  ( 0.8660254037844443697, 0.000000000000000000, 0.4999999999999901745 ) ) ;
#22084 = CARTESIAN_POINT ( 'NONE',  ( -0.2819296736111110979, 4.575083333409199149, 0.000000000000000000 ) ) ;
#22085 = SHAPE_DEFINITION_REPRESENTATION ( #3297, #18521 ) ;
#22086 = EDGE_CURVE ( 'NONE', #8442, #6063, #13564, .T. ) ;
#22087 = DIRECTION ( 'NONE',  ( 0.000000000000000000, 0.000000000000000000, -1.000000000000000000 ) ) ;
#22088 = CARTESIAN_POINT ( 'NONE',  ( -0.2206173157302028787, 0.4347222220704892726, 0.2206173157302027954 ) ) ;
#22089 = CARTESIAN_POINT ( 'NONE',  ( -0.1167790944451422702, 0.5666666665908001166, -0.2819296736111110424 ) ) ;
#22090 = EDGE_LOOP ( 'NONE', ( #7457, #4327, #10417, #7403 ) ) ;
#22091 = EDGE_LOOP ( 'NONE', ( #13333, #3014, #18941, #23934 ) ) ;
#22092 = CARTESIAN_POINT ( 'NONE',  ( 0.2819296736111110424, 0.2749999999241333204, -0.1167790944451423119 ) ) ;
#22093 = DIRECTION ( 'NONE',  ( -0.000000000000000000, -1.000000000000000000, -0.000000000000000000 ) ) ;
#22094 = CARTESIAN_POINT ( 'NONE',  ( 2.986000000000000210, 2.740000000000000213, 0.000000000000000000 ) ) ;
#22095 = CARTESIAN_POINT ( 'NONE',  ( 0.3999999999999999667, -0.09642857142857144681, -0.1299678784931625475 ) ) ;
#22096 = CARTESIAN_POINT ( 'NONE',  ( -0.1306872919485614903, 0.3155070326520293400, -0.003680555555554630362 ) ) ;
#22097 = CARTESIAN_POINT ( 'NONE',  ( -1.910449006669871087E-17, 4.203555555555555046, -0.3119999999999999996 ) ) ;
#22098 = CARTESIAN_POINT ( 'NONE',  ( -0.2563606228057540570, 3.885658506346372665, -0.1778292439628233468 ) ) ;
#22099 = CARTESIAN_POINT ( 'NONE',  ( 0.1167790944451423257, 0.04583333325746669074, -0.2819296736111110424 ) ) ;
#22100 = CARTESIAN_POINT ( 'NONE',  ( 0.2819296736111110979, 4.613277777853643791, 0.1167790944451422425 ) ) ;
#22101 = AXIS2_PLACEMENT_3D ( 'NONE', #16206, #14372, #13901 ) ;
#22102 = CARTESIAN_POINT ( 'NONE',  ( 0.3236067977499790249, 0.04107142837634378957, -0.2351141009169892826 ) ) ;
#22103 = CARTESIAN_POINT ( 'NONE',  ( 0.0002615309095209263448, 4.543825908977736638, -0.3119999184752035859 ) ) ;
#22104 = CARTESIAN_POINT ( 'NONE',  ( -0.1167790944451423257, 5.134111111186976828, -0.2819296736111110424 ) ) ;
#22105 = CARTESIAN_POINT ( 'NONE',  ( 0.2819296736111111534, 4.432722222298088433, 0.1167790944451422563 ) ) ;
#22106 = CARTESIAN_POINT ( 'NONE',  ( 0.1262412304268583363, 3.762410328379145685, -0.2858544259516618835 ) ) ;
#22107 = CARTESIAN_POINT ( 'NONE',  ( -0.2206173157302028787, 0.4902777776260447973, 0.2206173157302027954 ) ) ;
#22108 = B_SPLINE_CURVE_WITH_KNOTS ( 'NONE', 3,
 ( #23901, #10768, #20384, #7454, #3432, #22324, #20504, #5748, #18194, #1611, #7220, #23781, #7103, #14541, #5258, #12729, #20145, #10885, #18314, #22809, #13570, #15381, #2219, #11607, #4392, #9896, #2457, #11729, #19268, #6100, #10023, #494, #13442, #15259, #738, #18791, #17210, #2573, #17445, #11854, #23039, #8167, #22572, #22689, #19037, #5979, #11484, #20978, #4275, #15621, #6343, #2340, #7696, #2086, #15142, #9775, #13796, #22926, #3919, #20861 ),
 .UNSPECIFIED., .F., .F.,
 ( 4, 2, 2, 1, 1, 2, 2, 1, 1, 2, 2, 2, 2, 2, 2, 2, 2, 2, 2, 1, 2, 2, 2, 2, 2, 1, 1, 2, 2, 1, 1, 1, 1, 1, 2, 4 ),
 ( 0.7590242753740639170, 0.7601283167772955318, 0.7612323581805270356, 0.7613703633559310013, 0.7614048646497819650, 0.7614134899732447614, 0.7614221152967074469, 0.7614393659436329287, 0.7615083685313349671, 0.7617843788821428985, 0.7623363995837586504, 0.7634404409869903763, 0.7656485237934537169, 0.7678566065999170576, 0.7689606480031487834, 0.7700646894063803982, 0.7722727722128437389, 0.7725487825636516703, 0.7726177851513537087, 0.7726867877390556361, 0.7728247929144596018, 0.7733768136160754647, 0.7744808550193070795, 0.7755848964225388054, 0.7761369171241545573, 0.7762749222995585230, 0.7763094235934094867, 0.7763266742403350795, 0.7763439248872605614, 0.7764129274749624887, 0.7765509326503664544, 0.7766199352380684928, 0.7766544365319194565, 0.7766716871788449383, 0.7766803125023076237, 0.7766889378257704202 ),
 .UNSPECIFIED. ) ;
#22109 = CARTESIAN_POINT ( 'NONE',  ( 0.2856353109896033193, 3.915016894130901814, 0.1313266209029238241 ) ) ;
#22110 = CARTESIAN_POINT ( 'NONE',  ( -0.2206173157302028232, 4.217444444596176290, -0.2206173157302028232 ) ) ;
#22111 = CARTESIAN_POINT ( 'NONE',  ( -0.2819296736111110424, 4.481333333409199149, 0.1167790944451424923 ) ) ;
#22112 = CARTESIAN_POINT ( 'NONE',  ( -0.1167790944451423257, 3.842444444520309865, -0.2819296736111110424 ) ) ;
#22113 = ADVANCED_FACE ( 'NONE', ( #16219 ), #6582, .T. ) ;
#22114 = VERTEX_POINT ( 'NONE', #19626 ) ;
#22115 = AXIS2_PLACEMENT_3D ( 'NONE', #18999, #13643, #4114 ) ;
#22116 = ORIENTED_EDGE ( 'NONE', *, *, #22086, .F. ) ;
#22117 = CALENDAR_DATE ( 2026, 7, 10 ) ;
#22118 = EDGE_CURVE ( 'NONE', #5409, #11982, #3766, .T. ) ;
#22119 = VERTEX_POINT ( 'NONE', #7309 ) ;
#22120 = CARTESIAN_POINT ( 'NONE',  ( 0.3119999999999999996, 0.2368055554038226151, -0.1292346314604056468 ) ) ;
#22121 = CARTESIAN_POINT ( 'NONE',  ( 0.000000000000000000, 3.738758431839877614E-19, 0.4425000000000000044 ) ) ;
#22122 = CARTESIAN_POINT ( 'NONE',  ( 1.910449006669871087E-17, 0.2541666666666663188, -0.3119999999999999996 ) ) ;
#22123 = LINE ( 'NONE', #23946, #12832 ) ;
#22124 = ORIENTED_EDGE ( 'NONE', *, *, #5635, .F. ) ;
#22125 = CARTESIAN_POINT ( 'NONE',  ( -6.979263641208234666E-17, 0.06517857133102902822, 0.3799334167787516980 ) ) ;
#22126 = APPLICATION_CONTEXT ( 'configuration controlled 3d designs of mechanical parts and assemblies' ) ;
#22127 = CARTESIAN_POINT ( 'NONE',  ( 0.2980859225763422549, 5.088325808746541057, -0.09136059965523930793 ) ) ;
#22128 = CARTESIAN_POINT ( 'NONE',  ( 0.2764156081756483641, 0.1144950937579610056, 0.1751388888888914530 ) ) ;
#22129 = CARTESIAN_POINT ( 'NONE',  ( -0.1167790944451423257, 4.286888888964754507, -0.2819296736111110424 ) ) ;
#22130 = CARTESIAN_POINT ( 'NONE',  ( -0.1993543840281266355, 5.082027777853643791, 0.1993543840281267465 ) ) ;
#22131 = EDGE_CURVE ( 'NONE', #23062, #2535, #20353, .T. ) ;
#22132 = CARTESIAN_POINT ( 'NONE',  ( -0.4687500000000004996, -0.1740109699597049420, 0.07813294176666467361 ) ) ;
#22133 = CARTESIAN_POINT ( 'NONE',  ( -0.3086600503652839889, 4.225649461085167147, 0.04553437359818874458 ) ) ;
#22134 = CARTESIAN_POINT ( 'NONE',  ( -0.3119999999999998885, 3.943138888888888527, 0.1292346314604058410 ) ) ;
#22135 = AXIS2_PLACEMENT_3D ( 'NONE', #5170, #12636, #20056 ) ;
#22136 = CARTESIAN_POINT ( 'NONE',  ( -0.1292346314604056745, 4.880638889040620931, -0.3119999999999999996 ) ) ;
#22137 = CARTESIAN_POINT ( 'NONE',  ( -0.2819296736111110979, 5.200083333409199149, 0.000000000000000000 ) ) ;
#22138 = EDGE_CURVE ( 'NONE', #13516, #21481, #21244, .T. ) ;
#22139 = EDGE_CURVE ( 'NONE', #6959, #21793, #7189, .T. ) ;
#22140 = CARTESIAN_POINT ( 'NONE',  ( 0.5097595264191668862, 2.291712385858714285, -0.6667552972947643486 ) ) ;
#22141 = EDGE_LOOP ( 'NONE', ( #671, #20952, #23580, #10316, #18580 ) ) ;
#22142 = CARTESIAN_POINT ( 'NONE',  ( 0.2742360776605723416, -0.1498359893662102316, 0.4241666666666772390 ) ) ;
#22143 = CARTESIAN_POINT ( 'NONE',  ( -0.2260933988346537915, 0.05608587455741884109, 0.2058197434722169872 ) ) ;
#22144 = ORIENTED_EDGE ( 'NONE', *, *, #3042, .F. ) ;
#22145 = EDGE_CURVE ( 'NONE', #9048, #22560, #14878, .T. ) ;
#22146 = CARTESIAN_POINT ( 'NONE',  ( -0.2230971623002953874, 0.2230971623002954152, 0.1699305555555582770 ) ) ;
#22147 = CARTESIAN_POINT ( 'NONE',  ( -1.726321361862525858E-17, 5.005638888964754507, -0.2819296736111110979 ) ) ;
#22148 = CIRCLE ( 'NONE', #8518, 0.3525000000000007017 ) ;
#22149 = CARTESIAN_POINT ( 'NONE',  ( 0.3296559951169310554, -0.3509388998445404639, 0.4107594315541606700 ) ) ;
#22150 = DIRECTION ( 'NONE',  ( 0.000000000000000000, 0.000000000000000000, -1.000000000000000000 ) ) ;
#22151 = ORIENTED_EDGE ( 'NONE', *, *, #1550, .F. ) ;
#22152 = CARTESIAN_POINT ( 'NONE',  ( -0.2819296736111111534, 0.1916666665908000056, 0.1167790944451422563 ) ) ;
#22153 = CARTESIAN_POINT ( 'NONE',  ( 0.1954553509668047195, 0.1954553509668046085, 0.2966666666666701313 ) ) ;
#22154 = CARTESIAN_POINT ( 'NONE',  ( -0.1993543840281266910, 4.915361111186976828, -0.1993543840281266910 ) ) ;
#22155 = CARTESIAN_POINT ( 'NONE',  ( 0.3001226394952070664, 4.471964646715294478, 0.08541954505744529802 ) ) ;
#22156 = ADVANCED_FACE ( 'NONE', ( #14759 ), #2169, .F. ) ;
#22157 = CARTESIAN_POINT ( 'NONE',  ( 0.2819296736111110979, 4.821611111186976828, 0.1167790944451422425 ) ) ;
#22158 = CARTESIAN_POINT ( 'NONE',  ( -0.4581189881604794678, 0.2644951211353315235, 0.3941886329748525153 ) ) ;
#22159 = DIRECTION ( 'NONE',  ( -1.000000000000000000, 0.000000000000000000, 0.000000000000000000 ) ) ;
#22160 = CARTESIAN_POINT ( 'NONE',  ( 0.2206173157302028787, 4.571611111111110404, 0.2206173157302027954 ) ) ;
#22161 = CARTESIAN_POINT ( 'NONE',  ( -0.3125000000000010547, 0.1294417382415911921, 0.3348611111111147731 ) ) ;
#22162 = CARTESIAN_POINT ( 'NONE',  ( -0.2206173157302028232, 4.766055555555554157, -0.2206173157302028232 ) ) ;
#22163 = CARTESIAN_POINT ( 'NONE',  ( 0.1167790944451424506, 4.092444444520309865, 0.2819296736111110424 ) ) ;
#22164 = DIRECTION ( 'NONE',  ( -0.000000000000000000, -1.000000000000000000, -0.000000000000000000 ) ) ;
#22165 = CARTESIAN_POINT ( 'NONE',  ( 0.2963340753493131641, 4.032741672258961074, -0.09762241780008150405 ) ) ;
#22166 = FACE_OUTER_BOUND ( 'NONE', #7061, .T. ) ;
#22167 = ORIENTED_EDGE ( 'NONE', *, *, #209, .F. ) ;
#22168 = VECTOR ( 'NONE', #2868, 39.37007874015748854 ) ;
#22169 = CARTESIAN_POINT ( 'NONE',  ( 0.3125000000000009437, -0.1294417382415913309, 0.1404166666666687990 ) ) ;
#22170 = ORIENTED_EDGE ( 'NONE', *, *, #525, .T. ) ;
#22171 = PLANE ( 'NONE',  #10708 ) ;
#22172 = EDGE_CURVE ( 'NONE', #20467, #6926, #20591, .T. ) ;
#22173 = EDGE_CURVE ( 'NONE', #412, #18852, #1580, .T. ) ;
#22174 = DIRECTION ( 'NONE',  ( -0.5000000000000012212, -0.8660254037844380415, 0.000000000000000000 ) ) ;
#22175 = CARTESIAN_POINT ( 'NONE',  ( 0.1144950937579609085, -0.2764156081756484751, 0.3279166666666704089 ) ) ;
#22176 = DIRECTION ( 'NONE',  ( -3.169619151431772953E-17, -0.9659258262890682012, -0.2588190451025213501 ) ) ;
#22177 = CYLINDRICAL_SURFACE ( 'NONE', #5045, 0.7500000000000001110 ) ;
#22178 = CARTESIAN_POINT ( 'NONE',  ( -0.1116596296178200276, 0.3473214284738860846, 0.3436530038418508792 ) ) ;
#22179 = CIRCLE ( 'NONE', #14810, 0.2499999999999999722 ) ;
#22180 = CARTESIAN_POINT ( 'NONE',  ( 0.1993543840281266355, 0.3062499999241333759, 0.1993543840281267465 ) ) ;
#22181 = DIRECTION ( 'NONE',  ( -1.000000000000000000, 0.000000000000000000, -0.000000000000000000 ) ) ;
#22182 = DIRECTION ( 'NONE',  ( 0.000000000000000000, 0.000000000000000000, -1.000000000000000000 ) ) ;
#22183 = CARTESIAN_POINT ( 'NONE',  ( -0.1079887943494003133, 0.1837715311241617522, -0.7422780453074593332 ) ) ;
#22184 = CARTESIAN_POINT ( 'NONE',  ( -0.2764156081756484196, 1.692557448933383907E-17, -0.1269444444444443043 ) ) ;
#22185 = EDGE_LOOP ( 'NONE', ( #17181, #1783, #3834, #9005, #2722, #21258 ) ) ;
#22186 = VERTEX_POINT ( 'NONE', #18282 ) ;
#22187 = CARTESIAN_POINT ( 'NONE',  ( -0.3004112128421244088, 5.107488232101096592, 0.07954157393797596509 ) ) ;
#22188 = CYLINDRICAL_SURFACE ( 'NONE', #3911, 0.3119999999999999996 ) ;
#22189 = CARTESIAN_POINT ( 'NONE',  ( 0.2206173157302027676, 0.01111111111111077500, 0.2206173157302028787 ) ) ;
#22190 = CARTESIAN_POINT ( 'NONE',  ( 0.1167790944451422702, 3.904944444520310753, -0.2819296736111110424 ) ) ;
#22191 = CARTESIAN_POINT ( 'NONE',  ( 0.2233192592356399997, 0.2366071427596004029, -0.3073725909049500049 ) ) ;
#22192 = ORIENTED_EDGE ( 'NONE', *, *, #1278, .F. ) ;
#22193 = CARTESIAN_POINT ( 'NONE',  ( -1.726321361862525858E-17, 4.408416666742533074, -0.2819296736111110979 ) ) ;
#22194 = CARTESIAN_POINT ( 'NONE',  ( 0.4749999999999999778, 3.575000000000000622, 2.908536147974959276E-17 ) ) ;
#22195 = DIRECTION ( 'NONE',  ( -0.000000000000000000, -1.000000000000000000, -0.000000000000000000 ) ) ;
#22196 = ORIENTED_EDGE ( 'NONE', *, *, #3824, .T. ) ;
#22197 = CARTESIAN_POINT ( 'NONE',  ( 0.3110112520880878306, 4.362073312222188193, 0.04245179714123451659 ) ) ;
#22198 = CARTESIAN_POINT ( 'NONE',  ( -0.1167790944451423535, 5.029944444520310753, 0.2819296736111110424 ) ) ;
#22199 = AXIS2_PLACEMENT_3D ( 'NONE', #18626, #1919, #9363 ) ;
#22200 = CARTESIAN_POINT ( 'NONE',  ( -0.1331303419516291220, 5.146900442876030546, -0.2730306959456248461 ) ) ;
#22201 = VECTOR ( 'NONE', #14957, 39.37007874015748854 ) ;
#22202 = CARTESIAN_POINT ( 'NONE',  ( -7.000945310522701902E-17, 0.2303571426620580065, 0.3999999999999999667 ) ) ;
#22203 = DIRECTION ( 'NONE',  ( -0.000000000000000000, -1.000000000000000000, -0.000000000000000000 ) ) ;
#22204 = CARTESIAN_POINT ( 'NONE',  ( -0.1993543840281266355, 4.748694444520309865, 0.1993543840281267465 ) ) ;
#22205 = COORDINATED_UNIVERSAL_TIME_OFFSET ( 0, 0, .AHEAD. ) ;
#22206 = CARTESIAN_POINT ( 'NONE',  ( -0.2206173157302027676, 4.779944444444443441, 0.2206173157302028787 ) ) ;
#22207 = CARTESIAN_POINT ( 'NONE',  ( 0.3120000000000000551, 4.908416666666665762, 0.1292346314604056190 ) ) ;
#22208 = CARTESIAN_POINT ( 'NONE',  ( -0.2819296736111110979, 0.4104166665908000056, -3.452642723725051716E-17 ) ) ;
#22209 = ORIENTED_EDGE ( 'NONE', *, *, #18127, .F. ) ;
#22210 = CARTESIAN_POINT ( 'NONE',  ( -0.1167790944451424368, 0.2541666665908000056, 0.2819296736111110424 ) ) ;
#22211 = CARTESIAN_POINT ( 'NONE',  ( -1.910449006669871087E-17, 4.314666666666665762, -0.3119999999999999996 ) ) ;
#22212 = CARTESIAN_POINT ( 'NONE',  ( -0.2845704250721091122, 5.201214412163930767, -0.01070544790218683727 ) ) ;
#22213 = CARTESIAN_POINT ( 'NONE',  ( 0.3613381517857143232, 0.4223214284738860957, 0.000000000000000000 ) ) ;
#22214 = CARTESIAN_POINT ( 'NONE',  ( 0.000000000000000000, 0.3155070326520292845, -0.007152777777776874076 ) ) ;
#22215 = CARTESIAN_POINT ( 'NONE',  ( -0.3853713378992620897, -0.3187716316911694547, 0.07807775719020886018 ) ) ;
#22216 = VECTOR ( 'NONE', #10183, 39.37007874015748143 ) ;
#22217 = CARTESIAN_POINT ( 'NONE',  ( 0.4450000000000002842, 2.665000000000000036, -2.591000000000000192 ) ) ;
#22218 = CARTESIAN_POINT ( 'NONE',  ( 0.2819296736111110979, -0.02013888896475552262, 0.000000000000000000 ) ) ;
#22219 = VECTOR ( 'NONE', #4609, 39.37007874015748143 ) ;
#22220 = CARTESIAN_POINT ( 'NONE',  ( 0.1167790944451424368, 4.439666666742532186, 0.2819296736111110424 ) ) ;
#22221 = CARTESIAN_POINT ( 'NONE',  ( -0.1236067977499790416, 0.01249999980491522077, 0.3804226065180614236 ) ) ;
#22222 = CARTESIAN_POINT ( 'NONE',  ( 0.1728547196185014345, 4.521197801589692311, 0.2619698204964887034 ) ) ;
#22223 = CARTESIAN_POINT ( 'NONE',  ( 0.1167790944451422702, 5.127166666742532186, -0.2819296736111110424 ) ) ;
#22224 = CARTESIAN_POINT ( 'NONE',  ( 0.2819296736111110979, 4.384111111186976828, -0.1167790944451423396 ) ) ;
#22225 = CARTESIAN_POINT ( 'NONE',  ( 0.1007954511899375599, 4.929790153955178056, -0.2959789403773529504 ) ) ;
#22226 = CARTESIAN_POINT ( 'NONE',  ( 0.000000000000000000, 0.1799999999999999933, 0.000000000000000000 ) ) ;
#22227 = APPROVAL ( #21372, 'UNSPECIFIED' ) ;
#22228 = CARTESIAN_POINT ( 'NONE',  ( 0.1292346314604058410, 4.019527777929511103, 0.3119999999999998885 ) ) ;
#22229 = EDGE_CURVE ( 'NONE', #13735, #8250, #22416, .T. ) ;
#22230 = CARTESIAN_POINT ( 'NONE',  ( 0.1167790944451422702, 4.516055555631421470, -0.2819296736111110979 ) ) ;
#22231 =( BOUNDED_CURVE ( )  B_SPLINE_CURVE ( 2, ( #20963, #13549, #11959, #13775, #13421, #7908, #12076, #11590, #23131 ),
 .UNSPECIFIED., .F., .T. ) 
 B_SPLINE_CURVE_WITH_KNOTS ( ( 3, 2, 2, 2, 3 ),
 ( 0.1562500000000000278, 0.1666666666666667407, 0.1770833333333333703, 0.1875000000000000000, 0.1979166666666667129 ),
 .UNSPECIFIED. ) 
 CURVE ( )  GEOMETRIC_REPRESENTATION_ITEM ( )  RATIONAL_B_SPLINE_CURVE ( ( 0.9999999999999997780, 0.9238795325112869605, 1.000000000000000000, 0.9238795325112867385, 1.000000000000000000, 0.9238795325112867385, 1.000000000000000000, 0.9238795325112869605, 0.9999999999999997780 ) ) 
 REPRESENTATION_ITEM ( '' )  );
#22232 =( BOUNDED_SURFACE ( )  B_SPLINE_SURFACE ( 3, 2, ( 
 ( #13634, #17159, #9601 ),
 ( #21052, #13160, #449 ),
 ( #22876, #8001, #19218 ),
 ( #15331, #13276, #11313 ),
 ( #20694, #15210, #3984 ),
 ( #18745, #4342, #9479 ) ),
 .UNSPECIFIED., .F., .F., .F. ) 
 B_SPLINE_SURFACE_WITH_KNOTS ( ( 4, 2, 4 ),
 ( 3, 3 ),
 ( 0.001790663949227913349, 0.002289857484343687730, 0.002789051019459461676 ),
 ( 0.000000000000000000, 1.000000000000000000 ),
 .UNSPECIFIED. ) 
 GEOMETRIC_REPRESENTATION_ITEM ( )  RATIONAL_B_SPLINE_SURFACE ( (
 ( 1.000000000000000000, 0.8285407536241355952, 1.000000000000000000),
 ( 1.000000000000000000, 0.8382697314792180165, 1.000000000000000000),
 ( 1.000000000000000000, 0.8433836253084626700, 1.000000000000000000),
 ( 1.000000000000000000, 0.8433992480894149102, 1.000000000000000000),
 ( 1.000000000000000000, 0.8382827608170251299, 1.000000000000000000),
 ( 1.000000000000000000, 0.8285407536241035098, 1.000000000000000000) ) ) 
 REPRESENTATION_ITEM ( '' )  SURFACE ( )  );
#22233 = CARTESIAN_POINT ( 'NONE',  ( 5.178964085587577574E-17, 3.866750000075865668, 0.2819296736111110979 ) ) ;
#22234 = ORIENTED_EDGE ( 'NONE', *, *, #13200, .T. ) ;
#22235 = PERSON_AND_ORGANIZATION_ROLE ( 'creator' ) ;
#22236 = CARTESIAN_POINT ( 'NONE',  ( 0.1111235690150410432, -0.2883545979860924202, 0.4202375072062948802 ) ) ;
#22237 = DIRECTION ( 'NONE',  ( 2.775557561562891967E-17, 0.7071067811865475727, 0.7071067811865474617 ) ) ;
#22238 = CARTESIAN_POINT ( 'NONE',  ( 0.000000000000000000, 0.06249999999999967387, 0.000000000000000000 ) ) ;
#22239 = ORIENTED_EDGE ( 'NONE', *, *, #10985, .F. ) ;
#22240 = CARTESIAN_POINT ( 'NONE',  ( 0.2206173157302027676, 0.4486111109593781676, 0.2206173157302028787 ) ) ;
#22241 = DIRECTION ( 'NONE',  ( 0.000000000000000000, 1.000000000000000000, 0.000000000000000000 ) ) ;
#22242 = CARTESIAN_POINT ( 'NONE',  ( -0.2270342100380514649, 3.717753562207886997, -0.2143185460272691856 ) ) ;
#22243 = CARTESIAN_POINT ( 'NONE',  ( 0.2923287055106771337, -0.07053571438325667575, -0.2123892367102620249 ) ) ;
#22244 = CARTESIAN_POINT ( 'NONE',  ( 0.000000000000000000, 0.000000000000000000, -0.01143517789850382292 ) ) ;
#22245 = VERTEX_POINT ( 'NONE', #5719 ) ;
#22246 = EDGE_LOOP ( 'NONE', ( #1767, #1974, #18779, #19809 ) ) ;
#22247 = CARTESIAN_POINT ( 'NONE',  ( -0.1116596296178199582, 0.1044642856167433131, -0.3436530038418508792 ) ) ;
#22248 = ORIENTED_EDGE ( 'NONE', *, *, #239, .F. ) ;
#22249 = CARTESIAN_POINT ( 'NONE',  ( 0.2716150497474701941, 5.090361019658427466, -0.1537593218455965693 ) ) ;
#22250 = B_SPLINE_CURVE_WITH_KNOTS ( 'NONE', 3,
 ( #19261, #6214, #2683, #11600, #21336, #17075, #10133, #8160, #367, #21093 ),
 .UNSPECIFIED., .F., .F.,
 ( 4, 2, 2, 2, 4 ),
 ( 0.000000000000000000, 0.003270554913819860229, 0.006541109827639720459, 0.009811664741459580688, 0.01308221965527943745 ),
 .UNSPECIFIED. ) ;
#22251 = CARTESIAN_POINT ( 'NONE',  ( 0.1144950937579611444, 0.2764156081756483641, 0.3487500000000040012 ) ) ;
#22252 = EDGE_CURVE ( 'NONE', #7381, #5448, #22295, .T. ) ;
#22253 = CARTESIAN_POINT ( 'NONE',  ( -0.1167790944451423257, 4.175777777853643791, -0.2819296736111110424 ) ) ;
#22254 = CARTESIAN_POINT ( 'NONE',  ( 0.2819296736111111534, 5.043833333409199149, 0.1167790944451422563 ) ) ;
#22255 = CARTESIAN_POINT ( 'NONE',  ( 0.3065849364905491314, 4.945545817829770315E-15, 0.4182516031572158233 ) ) ;
#22256 = CARTESIAN_POINT ( 'NONE',  ( -0.3119999999999999996, 0.3687499998482670627, -0.1292346314604056745 ) ) ;
#22257 = DIRECTION ( 'NONE',  ( 0.000000000000000000, 0.000000000000000000, -1.000000000000000000 ) ) ;
#22258 = CARTESIAN_POINT ( 'NONE',  ( 0.1292346314604056190, 4.818138889040620931, -0.3119999999999999996 ) ) ;
#22259 = EDGE_CURVE ( 'NONE', #14703, #2366, #9255, .T. ) ;
#22260 = CARTESIAN_POINT ( 'NONE',  ( 0.1993543840281266633, 5.123694444520309865, -0.1993543840281266910 ) ) ;
#22261 = FACE_OUTER_BOUND ( 'NONE', #19029, .T. ) ;
#22262 = CARTESIAN_POINT ( 'NONE',  ( -0.3613381517857143232, 0.1687499999024575370, -0.1174058825155741143 ) ) ;
#22263 = CARTESIAN_POINT ( 'NONE',  ( 0.3125000000000000000, -5.740531871003217465E-17, 0.2063888888888918416 ) ) ;
#22264 = VERTEX_POINT ( 'NONE', #18641 ) ;
#22265 = APPROVAL_STATUS ( 'not_yet_approved' ) ;
#22266 = CARTESIAN_POINT ( 'NONE',  ( -0.3155070326520293400, 0.1306872919485614903, 0.1734027777777805146 ) ) ;
#22267 = CARTESIAN_POINT ( 'NONE',  ( -0.1167790944451423535, 5.085500000075866112, 0.2819296736111110424 ) ) ;
#22268 = ORIENTED_EDGE ( 'NONE', *, *, #3360, .T. ) ;
#22269 = CARTESIAN_POINT ( 'NONE',  ( 0.2537239961729473303, -0.3947782598749511318, 0.4289714952839356332 ) ) ;
#22270 = EDGE_CURVE ( 'NONE', #12390, #13943, #12293, .T. ) ;
#22271 = DIRECTION ( 'NONE',  ( -0.000000000000000000, 1.000000000000000000, -0.000000000000000000 ) ) ;
#22272 = EDGE_CURVE ( 'NONE', #8463, #14698, #1931, .T. ) ;
#22273 = EDGE_CURVE ( 'NONE', #5886, #280, #19286, .T. ) ;
#22274 = CARTESIAN_POINT ( 'NONE',  ( 0.2819296736111110424, 0.3791666665908000611, 0.1167790944451424923 ) ) ;
#22275 = CARTESIAN_POINT ( 'NONE',  ( -0.1144950937579609779, 0.2764156081756484196, 0.2515277777777809587 ) ) ;
#22276 = CARTESIAN_POINT ( 'NONE',  ( -0.2819296736111110979, 5.033416666742532186, 0.000000000000000000 ) ) ;
#22277 = CARTESIAN_POINT ( 'NONE',  ( -0.4795759075923630710, -0.04327657950267028292, 0.07439896364134127027 ) ) ;
#22278 = CARTESIAN_POINT ( 'NONE',  ( -1.726321361862525858E-17, 4.894527777853642903, -0.2819296736111110979 ) ) ;
#22279 = DIRECTION ( 'NONE',  ( -0.4999999999999916178, 0.000000000000000000, -0.8660254037844433705 ) ) ;
#22280 = CARTESIAN_POINT ( 'NONE',  ( -0.2082794372640225100, 5.206640035683668621, 0.1900105704308308607 ) ) ;
#22281 = CARTESIAN_POINT ( 'NONE',  ( -0.5116234456863466562, 2.661589509557312994, 2.693707776877850790 ) ) ;
#22282 = CARTESIAN_POINT ( 'NONE',  ( 0.000000000000000000, 6.000000000000000888, 0.000000000000000000 ) ) ;
#22283 = CARTESIAN_POINT ( 'NONE',  ( -0.3119999999999999996, 4.439666666666665762, 0.000000000000000000 ) ) ;
#22284 = CARTESIAN_POINT ( 'NONE',  ( -1.726321361862525858E-17, 3.950083333409199149, -0.2819296736111110979 ) ) ;
#22285 = CARTESIAN_POINT ( 'NONE',  ( -0.3119999999999999996, 4.213972222222222008, -0.1292346314604056468 ) ) ;
#22286 = ADVANCED_FACE ( 'NONE', ( #22055 ), #7072, .F. ) ;
#22287 = CARTESIAN_POINT ( 'NONE',  ( 0.1203817380124382053, 4.040418582577093076, -0.2885312214009505549 ) ) ;
#22288 = CARTESIAN_POINT ( 'NONE',  ( -0.1061085311203168874, 3.735219933786901425, 0.2934028053144311921 ) ) ;
#22289 = DIRECTION ( 'NONE',  ( -0.000000000000000000, -1.000000000000000000, -0.000000000000000000 ) ) ;
#22290 = VERTEX_POINT ( 'NONE', #20112 ) ;
#22291 = CARTESIAN_POINT ( 'NONE',  ( 0.000000000000000000, 0.1199999999999999956, 0.000000000000000000 ) ) ;
#22292 = CIRCLE ( 'NONE', #21898, 0.2501339745962155581 ) ;
#22293 = CARTESIAN_POINT ( 'NONE',  ( 0.01077313864395416584, 4.654635478660750891, -0.3118404384345617175 ) ) ;
#22294 = CARTESIAN_POINT ( 'NONE',  ( -0.2764156081756484196, 0.1144950937579609918, 0.2515277777777809587 ) ) ;
#22295 = LINE ( 'NONE', #1695, #16557 ) ;
#22296 = CARTESIAN_POINT ( 'NONE',  ( 0.4788451055546354973, 0.2690082051306184052, 0.04193467568257210065 ) ) ;
#22297 = CARTESIAN_POINT ( 'NONE',  ( -0.3613381517857143232, 0.3330357141881718497, -4.425116109941954795E-17 ) ) ;
#22298 = CARTESIAN_POINT ( 'NONE',  ( -0.2819296736111110979, 0.1777777777019111383, 0.1167790944451422425 ) ) ;
#22299 = CARTESIAN_POINT ( 'NONE',  ( 0.0005571238342427710811, 3.877151696567567196, -0.3119995739661102774 ) ) ;
#22300 = FACE_OUTER_BOUND ( 'NONE', #6730, .T. ) ;
#22301 = DIRECTION ( 'NONE',  ( -0.000000000000000000, 0.000000000000000000, -1.000000000000000000 ) ) ;
#22302 = CARTESIAN_POINT ( 'NONE',  ( 0.2764156081756484196, -5.077672346800151106E-17, -0.09916666666666629215 ) ) ;
#22303 = VERTEX_POINT ( 'NONE', #16577 ) ;
#22304 = ORIENTED_EDGE ( 'NONE', *, *, #9965, .T. ) ;
#22305 = CARTESIAN_POINT ( 'NONE',  ( 0.08808798601665612793, 3.066692553488282957, 3.256612888476066558 ) ) ;
#22306 = DIRECTION ( 'NONE',  ( 0.000000000000000000, 0.000000000000000000, -1.000000000000000000 ) ) ;
#22307 = CARTESIAN_POINT ( 'NONE',  ( 0.2206173157302027676, 0.06666666666666633267, 0.2206173157302028787 ) ) ;
#22308 = CARTESIAN_POINT ( 'NONE',  ( -0.1292346314604056745, 5.095916666666666650, -0.3119999999999999996 ) ) ;
#22309 = CARTESIAN_POINT ( 'NONE',  ( 2.326421213736078119E-17, 0.1723214284738861790, -0.3799334167787516425 ) ) ;
#22310 = CIRCLE ( 'NONE', #14528, 0.4062499999999995004 ) ;
#22311 = CARTESIAN_POINT ( 'NONE',  ( 0.2819296736111110979, 4.446611111186976828, 0.1167790944451422425 ) ) ;
#22312 = CARTESIAN_POINT ( 'NONE',  ( 0.1292346314604056745, 0.1326388887371559577, -0.3119999999999999996 ) ) ;
#22313 = CARTESIAN_POINT ( 'NONE',  ( 0.3236067977499790249, 0.3982142855192009057, -0.2351141009169892826 ) ) ;
#22314 = ORIENTED_EDGE ( 'NONE', *, *, #20792, .F. ) ;
#22315 = CARTESIAN_POINT ( 'NONE',  ( 0.1268833284183610299, 4.373501793580047092, -0.2854709177596411185 ) ) ;
#22316 = CARTESIAN_POINT ( 'NONE',  ( 0.2819296736111110979, 4.991750000075866112, -3.452642723725051716E-17 ) ) ;
#22317 = CARTESIAN_POINT ( 'NONE',  ( -0.2818813690555227458, 5.158154447605131310, 0.1035947188507469058 ) ) ;
#22318 =( LENGTH_UNIT ( ) NAMED_UNIT ( * ) SI_UNIT ( $, .METRE. ) );
#22319 = CARTESIAN_POINT ( 'NONE',  ( 0.4795759075923620163, -5.969813580926603513E-13, 0.07439896364136204532 ) ) ;
#22320 = DIRECTION ( 'NONE',  ( -0.6681584153635194978, 0.6681584153635199419, 0.3273051541876792481 ) ) ;
#22321 = CARTESIAN_POINT ( 'NONE',  ( -0.1993543840281266910, 4.679250000075866112, -0.1993543840281266910 ) ) ;
#22322 = APPROVAL_DATE_TIME ( #17209, #4198 ) ;
#22323 = AXIS2_PLACEMENT_3D ( 'NONE', #13876, #7445, #13076 ) ;
#22324 = CARTESIAN_POINT ( 'NONE',  ( -0.1456855345975412996, 4.067294776256560773, 0.2759172852803205567 ) ) ;
#22325 = DIRECTION ( 'NONE',  ( 0.8660254037844434816, 0.000000000000000000, 0.4999999999999913403 ) ) ;
#22326 = CARTESIAN_POINT ( 'NONE',  ( 0.2819296736111110979, 0.4937499999241333759, 0.000000000000000000 ) ) ;
#22327 = ORIENTED_EDGE ( 'NONE', *, *, #22555, .F. ) ;
#22328 = CARTESIAN_POINT ( 'NONE',  ( -0.2819296736111110424, 0.1847222221463555858, -0.1167790944451423396 ) ) ;
#22329 = CARTESIAN_POINT ( 'NONE',  ( -1.296004783052830448E-07, 4.710500003633881327, -0.3119999999999730766 ) ) ;
#22330 = CARTESIAN_POINT ( 'NONE',  ( -0.2611278098349356092, 5.204257314301414361, 0.1100826262484129597 ) ) ;
#22331 = CARTESIAN_POINT ( 'NONE',  ( -0.2472135954999579999, 0.3035714285714284921, 0.3402603233408159622 ) ) ;
#22332 = CYLINDRICAL_SURFACE ( 'NONE', #19820, 0.2500000000000000000 ) ;
#22333 = CARTESIAN_POINT ( 'NONE',  ( 0.4687500000000002220, -0.1742897399511009748, 0.3995693456591889459 ) ) ;
#22334 = DIRECTION ( 'NONE',  ( 0.000000000000000000, 0.000000000000000000, -1.000000000000000000 ) ) ;
#22335 = CARTESIAN_POINT ( 'NONE',  ( -0.1993543840281267465, 0.3479166665908000611, 0.1993543840281266633 ) ) ;
#22336 = CARTESIAN_POINT ( 'NONE',  ( -5.178964085587577574E-17, 0.02152777770191114173, 0.2819296736111110979 ) ) ;
#22337 = CARTESIAN_POINT ( 'NONE',  ( 0.1993543840281266633, 4.568138888964755395, -0.1993543840281266910 ) ) ;
#22338 = CARTESIAN_POINT ( 'NONE',  ( 0.1236067977499789861, -0.02321428590937048980, -0.3804226065180614236 ) ) ;
#22339 = FACE_OUTER_BOUND ( 'NONE', #222, .T. ) ;
#22340 = CARTESIAN_POINT ( 'NONE',  ( -0.1993543840281266355, 5.151472222298088433, 0.1993543840281267465 ) ) ;
#22341 = EDGE_CURVE ( 'NONE', #9981, #1934, #4555, .T. ) ;
#22342 = CARTESIAN_POINT ( 'NONE',  ( 0.1993543840281267465, 4.429250000075865223, 0.1993543840281266633 ) ) ;
#22343 = CARTESIAN_POINT ( 'NONE',  ( 0.04081965062135220479, 4.906194639886546582, 0.3120000089134554178 ) ) ;
#22344 = CARTESIAN_POINT ( 'NONE',  ( -0.3886563986012126493, 0.3298860868734690976, 0.06108838700204354683 ) ) ;
#22345 = CARTESIAN_POINT ( 'NONE',  ( -0.2206173157302027676, 4.064666666818398610, 0.2206173157302028787 ) ) ;
#22346 = VECTOR ( 'NONE', #10394, 39.37007874015748854 ) ;
#22347 = CARTESIAN_POINT ( 'NONE',  ( 0.1167790944451422702, 4.571611111186976828, -0.2819296736111110979 ) ) ;
#22348 = CARTESIAN_POINT ( 'NONE',  ( 0.3003475124358450099, 4.111524471938507119, -3.730379552481990491 ) ) ;
#22349 = CARTESIAN_POINT ( 'NONE',  ( -0.1850421345840768672, -0.2494223792523551642, -0.09928129690674993013 ) ) ;
#22350 = ORIENTED_EDGE ( 'NONE', *, *, #7665, .F. ) ;
#22351 = ORIENTED_EDGE ( 'NONE', *, *, #7888, .T. ) ;
#22352 = DATE_AND_TIME ( #5413, #13086 ) ;
#22353 = CARTESIAN_POINT ( 'NONE',  ( -0.1290798622871512646, 4.845609795294118172, 0.2840783873375067881 ) ) ;
#22354 = CARTESIAN_POINT ( 'NONE',  ( 2.986000000000000210, 2.664999999999999591, -2.541000000000000369 ) ) ;
#22355 = VERTEX_POINT ( 'NONE', #16932 ) ;
#22356 = CARTESIAN_POINT ( 'NONE',  ( -0.3119999999999999996, 0.4243055554038226429, -0.1292346314604056745 ) ) ;
#22357 = ORIENTED_EDGE ( 'NONE', *, *, #17520, .T. ) ;
#22358 = CARTESIAN_POINT ( 'NONE',  ( 0.1891708636127259202, 2.539511724522405989E-17, 0.3078630284654709781 ) ) ;
#22359 = FACE_OUTER_BOUND ( 'NONE', #7683, .T. ) ;
#22360 = CIRCLE ( 'NONE', #14191, 1.243000000000000105 ) ;
#22361 = CARTESIAN_POINT ( 'NONE',  ( 0.1116596296178199860, -0.06339285724039953052, -0.3436530038418508792 ) ) ;
#22362 = CARTESIAN_POINT ( 'NONE',  ( 0.2724977880658804863, 3.969733213627001156, 0.1573355931994520895 ) ) ;
#22363 = CC_DESIGN_PERSON_AND_ORGANIZATION_ASSIGNMENT ( #4388, #852, ( #8363 ) ) ;
#22364 = ORIENTED_EDGE ( 'NONE', *, *, #21127, .F. ) ;
#22365 = CARTESIAN_POINT ( 'NONE',  ( 0.1116596296178199860, 0.1687499999024575925, -0.3436530038418508792 ) ) ;
#22366 = EDGE_LOOP ( 'NONE', ( #1949, #19471, #19856, #21277 ) ) ;
#22367 = CARTESIAN_POINT ( 'NONE',  ( 0.01924054892003582498, 5.099521701092943893, -0.3108711954494297602 ) ) ;
#22368 = CARTESIAN_POINT ( 'NONE',  ( -0.1954553509668046640, 0.1954553509668046918, 0.3591666666666706864 ) ) ;
#22369 = CARTESIAN_POINT ( 'NONE',  ( 0.2819296736111110979, 4.154944444520309865, 0.1167790944451422425 ) ) ;
#22370 = CARTESIAN_POINT ( 'NONE',  ( -0.1167790944451423535, 5.029944444520308977, 0.2819296736111110979 ) ) ;
#22371 =( BOUNDED_CURVE ( )  B_SPLINE_CURVE ( 2, ( #18671, #18552, #9165, #16372, #23782, #22207, #7455, #23903, #5259 ),
 .UNSPECIFIED., .F., .F. ) 
 B_SPLINE_CURVE_WITH_KNOTS ( ( 3, 2, 2, 2, 3 ),
 ( 0.2232142857142854764, 0.2276785714285712858, 0.2321428571428570953, 0.2366071428571429047, 0.2410714285714287142 ),
 .UNSPECIFIED. ) 
 CURVE ( )  GEOMETRIC_REPRESENTATION_ITEM ( )  RATIONAL_B_SPLINE_CURVE ( ( 1.000000000000004219, 0.9238795325112825196, 1.000000000000000000, 0.9238795325112867385, 1.000000000000000000, 0.9238795325112867385, 1.000000000000000000, 0.9238795325112844070, 1.000000000000002442 ) ) 
 REPRESENTATION_ITEM ( '' )  );
#22372 = CARTESIAN_POINT ( 'NONE',  ( 0.2107770390570962993, -0.2008625216908654920, 0.4022918831151609531 ) ) ;
#22373 = CARTESIAN_POINT ( 'NONE',  ( 5.731347020009612645E-17, 4.842444444444443441, 0.3119999999999999996 ) ) ;
#22374 = CARTESIAN_POINT ( 'NONE',  ( 0.3119999999999999996, 3.852861111111110404, 0.1292346314604056190 ) ) ;
#22375 = CARTESIAN_POINT ( 'NONE',  ( -0.2206173157302028232, 4.661888889040620931, -0.2206173157302028232 ) ) ;
#22376 = CARTESIAN_POINT ( 'NONE',  ( 0.2819296736111110979, 5.172305555631421470, -3.452642723725051716E-17 ) ) ;
#22377 = LINE ( 'NONE', #187, #12476 ) ;
#22378 = CARTESIAN_POINT ( 'NONE',  ( 0.3613381517857143232, 0.2080357141881718774, 0.000000000000000000 ) ) ;
#22379 = AXIS2_PLACEMENT_3D ( 'NONE', #1782, #20321, #23968 ) ;
#22380 = CARTESIAN_POINT ( 'NONE',  ( 0.2732760442592158667, 0.03601662800317857738, -0.08586055624119162677 ) ) ;
#22381 = ORIENTED_EDGE ( 'NONE', *, *, #8670, .T. ) ;
#22382 = EDGE_CURVE ( 'NONE', #20541, #22410, #23169, .T. ) ;
#22383 = CALENDAR_DATE ( 2026, 7, 10 ) ;
#22384 = VERTEX_POINT ( 'NONE', #4123 ) ;
#22385 = CARTESIAN_POINT ( 'NONE',  ( 0.4675613926561236200, 0.2849392891917821302, 0.04271845132551801288 ) ) ;
#22386 = CARTESIAN_POINT ( 'NONE',  ( 0.2819296736111110979, 5.210500000075865223, 0.1167790944451422425 ) ) ;
#22387 = CC_DESIGN_APPROVAL ( #14786, ( #22007 ) ) ;
#22388 = CARTESIAN_POINT ( 'NONE',  ( 0.1993543840281266633, 3.957027777853643791, -0.1993543840281266910 ) ) ;
#22389 = CARTESIAN_POINT ( 'NONE',  ( 0.4593750000000004219, -0.2760455974562899262, 0.3779506566538943235 ) ) ;
#22390 = EDGE_CURVE ( 'NONE', #7867, #11483, #13537, .T. ) ;
#22391 = DIRECTION ( 'NONE',  ( 0.000000000000000000, 0.000000000000000000, -1.000000000000000000 ) ) ;
#22392 = CARTESIAN_POINT ( 'NONE',  ( -0.1144950937579609918, -0.2764156081756484196, 0.04319444444444596465 ) ) ;
#22393 = CARTESIAN_POINT ( 'NONE',  ( -0.2819296736111110979, 0.5180555554796888451, -0.1167790944451423396 ) ) ;
#22394 = CARTESIAN_POINT ( 'NONE',  ( 0.2764156081756484196, -5.077672346800151106E-17, 0.2341666666666696595 ) ) ;
#22395 = CARTESIAN_POINT ( 'NONE',  ( -0.1993543840281266355, 4.873694444520310753, 0.1993543840281267465 ) ) ;
#22396 = CARTESIAN_POINT ( 'NONE',  ( -0.2472135954999579999, 0.4374999998049151073, 0.3402603233408160732 ) ) ;
#22397 = VECTOR ( 'NONE', #22237, 39.37007874015748143 ) ;
#22398 = CARTESIAN_POINT ( 'NONE',  ( 5.178964085587577574E-17, 4.866750000075865223, 0.2819296736111110979 ) ) ;
#22399 = CARTESIAN_POINT ( 'NONE',  ( -0.3236067977499789694, 0.06249999980491519752, -0.2351141009169893104 ) ) ;
#22400 = DIRECTION ( 'NONE',  ( -0.000000000000000000, 1.000000000000000000, -0.000000000000000000 ) ) ;
#22401 = DIRECTION ( 'NONE',  ( 0.000000000000000000, 1.000000000000000000, 0.000000000000000000 ) ) ;
#22402 = CARTESIAN_POINT ( 'NONE',  ( 1.652041376866375977, 2.315961009048385755, -2.060610414248980504 ) ) ;
#22403 = CARTESIAN_POINT ( 'NONE',  ( 0.3119999999999999996, 4.463972222222222008, 0.1292346314604056190 ) ) ;
#22404 = CARTESIAN_POINT ( 'NONE',  ( 0.1167790944451424506, 3.814666666742532630, 0.2819296736111110424 ) ) ;
#22405 = CARTESIAN_POINT ( 'NONE',  ( 0.3119999999999999996, 0.3479166665149338589, -0.1292346314604056468 ) ) ;
#22406 = CARTESIAN_POINT ( 'NONE',  ( 0.2045172001623904168, 4.022406176792101107, 0.2356682906421939394 ) ) ;
#22407 = CARTESIAN_POINT ( 'NONE',  ( -0.09399142304410415538, 3.735586886565314124, 0.2976376820043376004 ) ) ;
#22408 = CC_DESIGN_APPROVAL ( #1200, ( #5667 ) ) ;
#22409 = DIRECTION ( 'NONE',  ( 0.8660254037844394848, 0.4999999999999983902, -0.000000000000000000 ) ) ;
#22410 = VERTEX_POINT ( 'NONE', #15348 ) ;
#22411 = FACE_OUTER_BOUND ( 'NONE', #22758, .T. ) ;
#22412 = ADVANCED_FACE ( 'NONE', ( #8018 ), #229, .F. ) ;
#22413 = AXIS2_PLACEMENT_3D ( 'NONE', #12162, #12277, #17747 ) ;
#22414 = CARTESIAN_POINT ( 'NONE',  ( 0.06359797816605802789, 4.153123496935264392, -0.3074626295701026191 ) ) ;
#22415 = CARTESIAN_POINT ( 'NONE',  ( 0.1954553509668046640, -0.1954553509668047195, 0.3869444444444487541 ) ) ;
#22416 = LINE ( 'NONE', #9380, #13079 ) ;
#22417 = ADVANCED_FACE ( 'NONE', ( #18888 ), #17180, .F. ) ;
#22418 = DIRECTION ( 'NONE',  ( 0.000000000000000000, 0.9659258262890680902, 0.2588190451025214611 ) ) ;
#22419 = ORIENTED_EDGE ( 'NONE', *, *, #7426, .F. ) ;
#22420 = APPROVAL_PERSON_ORGANIZATION ( #8674, #21485, #17954 ) ;
#22421 = CARTESIAN_POINT ( 'NONE',  ( 2.326421213736078119E-17, 0.2437499999024574926, -0.3799334167787516425 ) ) ;
#22422 = CARTESIAN_POINT ( 'NONE',  ( -0.2819296736111110424, 0.2263888888130222710, -0.1167790944451423396 ) ) ;
#22423 = CARTESIAN_POINT ( 'NONE',  ( 0.3038785920422452658, 3.861053045795140193, 0.08166846456136669929 ) ) ;
#22424 = CARTESIAN_POINT ( 'NONE',  ( 0.06335377612981453466, 0.04995520403538498966, -0.3999999999999999667 ) ) ;
#22425 = CARTESIAN_POINT ( 'NONE',  ( -0.1292346314604056190, 0.1465277777777774515, -0.3119999999999999996 ) ) ;
#22426 = CARTESIAN_POINT ( 'NONE',  ( -0.2764156081756484196, 1.692557448933383907E-17, -0.07138888888888829387 ) ) ;
#22427 = VERTEX_POINT ( 'NONE', #22896 ) ;
#22428 = DIRECTION ( 'NONE',  ( 0.000000000000000000, 1.000000000000000000, 0.000000000000000000 ) ) ;
#22429 = CARTESIAN_POINT ( 'NONE',  ( 0.1292346314604058410, 4.345916666666665762, 0.3119999999999998885 ) ) ;
#22430 = CARTESIAN_POINT ( 'NONE',  ( 0.1993543840281266355, 0.5840277777019111660, 0.1993543840281267465 ) ) ;
#22431 = CARTESIAN_POINT ( 'NONE',  ( -0.2206173157302028232, 5.266055555555555046, -0.2206173157302028232 ) ) ;
#22432 = CARTESIAN_POINT ( 'NONE',  ( 0.2233192592356399164, 0.2151785713310289949, 0.3073725909049500604 ) ) ;
#22433 = AXIS2_PLACEMENT_3D ( 'NONE', #11087, #18159, #10728 ) ;
#22434 = ORIENTED_EDGE ( 'NONE', *, *, #13653, .T. ) ;
#22435 = CARTESIAN_POINT ( 'NONE',  ( 0.1993543840281266633, 4.179250000075865223, -0.1993543840281266910 ) ) ;
#22436 = CARTESIAN_POINT ( 'NONE',  ( 5.731347020009612645E-17, 4.286888888888888083, 0.3119999999999999996 ) ) ;
#22437 = DIRECTION ( 'NONE',  ( 0.000000000000000000, 0.000000000000000000, 1.000000000000000000 ) ) ;
#22438 = ORIENTED_EDGE ( 'NONE', *, *, #22834, .F. ) ;
#22439 = CARTESIAN_POINT ( 'NONE',  ( 0.1236067977499789028, 0.3053571426620579898, 0.3804226065180614791 ) ) ;
#22440 = CARTESIAN_POINT ( 'NONE',  ( -0.2819296736111110979, 4.963972222298087544, 0.000000000000000000 ) ) ;
#22441 = CARTESIAN_POINT ( 'NONE',  ( -0.3124999999999989453, 0.1294417382415933293, 0.008472222222223593432 ) ) ;
#22442 = EDGE_CURVE ( 'NONE', #3065, #10673, #15116, .T. ) ;
#22443 = FACE_OUTER_BOUND ( 'NONE', #19821, .T. ) ;
#22444 = CARTESIAN_POINT ( 'NONE',  ( -0.1292346314604058410, 0.2229166666666663466, 0.3119999999999998885 ) ) ;
#22445 = AXIS2_PLACEMENT_3D ( 'NONE', #12447, #16332, #1693 ) ;
#22446 = CARTESIAN_POINT ( 'NONE',  ( -0.1167790944451423119, 4.675777777853642903, -0.2819296736111110979 ) ) ;
#22447 = CALENDAR_DATE ( 2026, 7, 10 ) ;
#22448 = EDGE_CURVE ( 'NONE', #10770, #16112, #10955, .T. ) ;
#22449 = CARTESIAN_POINT ( 'NONE',  ( -0.2206173157302028232, 4.766055555555554157, -0.2206173157302028232 ) ) ;
#22450 = DIRECTION ( 'NONE',  ( -0.8660254037844434816, 0.000000000000000000, 0.4999999999999916178 ) ) ;
#22451 = CARTESIAN_POINT ( 'NONE',  ( 0.1993543840281266355, 0.4868055554796889561, 0.1993543840281267465 ) ) ;
#22452 = ORIENTED_EDGE ( 'NONE', *, *, #8761, .F. ) ;
#22453 = ORIENTED_EDGE ( 'NONE', *, *, #9016, .F. ) ;
#22454 = CARTESIAN_POINT ( 'NONE',  ( -0.1167790944451422702, 0.1222222221463555858, -0.2819296736111110424 ) ) ;
#22455 = DIRECTION ( 'NONE',  ( 1.000000000000000000, 0.000000000000000000, 0.000000000000000000 ) ) ;
#22456 = PLANE ( 'NONE',  #9768 ) ;
#22457 = CARTESIAN_POINT ( 'NONE',  ( 0.3236067977499789694, 0.3214285714285713413, 0.2351141009169893659 ) ) ;
#22458 = CARTESIAN_POINT ( 'NONE',  ( 0.2230971623002954429, 0.2230971623002953319, -0.06965277777777736934 ) ) ;
#22459 = CARTESIAN_POINT ( 'NONE',  ( -0.09136153228684393279, -0.5015293579687629677, 0.06108838700204188843 ) ) ;
#22460 = DIRECTION ( 'NONE',  ( -1.000000000000000000, 0.000000000000000000, 0.000000000000000000 ) ) ;
#22461 = CARTESIAN_POINT ( 'NONE',  ( -0.2819296736111110979, 0.1708333332574666907, -0.1167790944451423396 ) ) ;
#22462 = CARTESIAN_POINT ( 'NONE',  ( 0.1167790944451423535, 0.08055555547968892838, 0.2819296736111110424 ) ) ;
#22463 = CARTESIAN_POINT ( 'NONE',  ( 0.1167790944451422702, 4.182722222298087544, -0.2819296736111110424 ) ) ;
#22464 = CARTESIAN_POINT ( 'NONE',  ( -0.3999999999999999667, -0.005357143052227637120, -0.1299678784931626030 ) ) ;
#22465 = CARTESIAN_POINT ( 'NONE',  ( -0.2819296736111110424, 4.807722222298088433, -0.1167790944451423119 ) ) ;
#22466 = CARTESIAN_POINT ( 'NONE',  ( 0.2819296736111110979, 4.495222222298087544, -0.1167790944451423396 ) ) ;
#22467 = LINE ( 'NONE', #5767, #17259 ) ;
#22468 = ORIENTED_EDGE ( 'NONE', *, *, #7039, .T. ) ;
#22469 = VECTOR ( 'NONE', #8292, 39.37007874015748854 ) ;
#22470 = ORIENTED_EDGE ( 'NONE', *, *, #5893, .T. ) ;
#22471 = FACE_OUTER_BOUND ( 'NONE', #16030, .T. ) ;
#22472 = CARTESIAN_POINT ( 'NONE',  ( -0.3119999999999999996, 4.057722222373953969, 0.000000000000000000 ) ) ;
#22473 = DIRECTION ( 'NONE',  ( 0.5000000000000037748, 0.000000000000000000, 0.8660254037844362651 ) ) ;
#22474 =( NAMED_UNIT ( * ) PLANE_ANGLE_UNIT ( ) SI_UNIT ( $, .RADIAN. ) );
#22475 = VERTEX_POINT ( 'NONE', #19237 ) ;
#22476 = VERTEX_POINT ( 'NONE', #15586 ) ;
#22477 = EDGE_CURVE ( 'NONE', #13943, #12390, #18126, .T. ) ;
#22478 = COORDINATED_UNIVERSAL_TIME_OFFSET ( 0, 0, .AHEAD. ) ;
#22479 = EDGE_CURVE ( 'NONE', #8797, #4857, #21313, .T. ) ;
#22480 = CARTESIAN_POINT ( 'NONE',  ( 0.3064624847683588005, -0.3533192024756442451, 0.4298724737630856274 ) ) ;
#22481 = CARTESIAN_POINT ( 'NONE',  ( -0.5116234456863258950, 1.487605717019675700, -2.710063190037627745 ) ) ;
#22482 = CARTESIAN_POINT ( 'NONE',  ( -0.3119999999999999996, 0.4798611109593782231, -0.1292346314604056745 ) ) ;
#22483 = VERTEX_POINT ( 'NONE', #12543 ) ;
#22484 = CARTESIAN_POINT ( 'NONE',  ( -0.4749999999999999778, 3.575000000000000622, -0.09499999999999995948 ) ) ;
#22485 = CARTESIAN_POINT ( 'NONE',  ( -4.974594353761572974E-07, 4.738258141874186258, 0.3119999999991586170 ) ) ;
#22486 = CARTESIAN_POINT ( 'NONE',  ( -0.2233192592356399442, -0.05267857152611380572, -0.3073725909049500049 ) ) ;
#22487 = CARTESIAN_POINT ( 'NONE',  ( 9.184850993605150903E-17, -3.937007874019685528E-05, -0.7500000000000001110 ) ) ;
#22488 = ORIENTED_EDGE ( 'NONE', *, *, #19439, .T. ) ;
#22489 = CARTESIAN_POINT ( 'NONE',  ( -0.3613381517857143232, 0.1901785713310290282, -4.425116109941954795E-17 ) ) ;
#22490 = EDGE_LOOP ( 'NONE', ( #19424, #533, #22209, #3300 ) ) ;
#22491 = CARTESIAN_POINT ( 'NONE',  ( 0.3635541710483937705, 0.08144582895160552838, -0.3889703289146366760 ) ) ;
#22492 = CARTESIAN_POINT ( 'NONE',  ( -0.2919176283147316697, 4.665648881694019146, -0.1102027081678718656 ) ) ;
#22493 = CARTESIAN_POINT ( 'NONE',  ( -0.1993543840281266355, 4.137583333409199149, 0.1993543840281267465 ) ) ;
#22494 = DIRECTION ( 'NONE',  ( -0.5000000000000037748, 0.000000000000000000, -0.8660254037844362651 ) ) ;
#22495 = DIRECTION ( 'NONE',  ( 0.000000000000000000, 0.000000000000000000, -1.000000000000000000 ) ) ;
#22496 = CARTESIAN_POINT ( 'NONE',  ( 0.2206173157302027954, 3.918833333333332281, -0.2206173157302028232 ) ) ;
#22497 = CARTESIAN_POINT ( 'NONE',  ( 0.1292346314604058410, 4.852861111262844140, 0.3119999999999998885 ) ) ;
#22498 = CARTESIAN_POINT ( 'NONE',  ( -0.2819296736111110424, 4.189666666742533074, 0.1167790944451424923 ) ) ;
#22499 = AXIS2_PLACEMENT_3D ( 'NONE', #7089, #20255, #3541 ) ;
#22500 = CARTESIAN_POINT ( 'NONE',  ( 0.000000000000000000, 3.066692553488282957, 0.2004988538245859597 ) ) ;
#22501 = VERTEX_POINT ( 'NONE', #23479 ) ;
#22502 = CARTESIAN_POINT ( 'NONE',  ( 0.1116596296178199027, 0.1937499999024575870, 0.3436530038418508792 ) ) ;
#22503 = CC_DESIGN_DATE_AND_TIME_ASSIGNMENT ( #6155, #13620, ( #10901 ) ) ;
#22504 = ORIENTED_EDGE ( 'NONE', *, *, #995, .F. ) ;
#22505 = ADVANCED_BREP_SHAPE_REPRESENTATION ( '', ( #17529, #9127 ), #12664 ) ;
#22506 = ORIENTED_EDGE ( 'NONE', *, *, #4559, .F. ) ;
#22507 = PERSON_AND_ORGANIZATION ( #15518, #2538 ) ;
#22508 = CARTESIAN_POINT ( 'NONE',  ( 0.4607735603406416525, 0.2757708160731982550, 0.04763592618480202295 ) ) ;
#22509 = CARTESIAN_POINT ( 'NONE',  ( 0.1993543840281266633, 5.054250000075865223, -0.1993543840281266910 ) ) ;
#22510 = CARTESIAN_POINT ( 'NONE',  ( -1.726321361862525858E-17, 3.852861111186976828, -0.2819296736111110979 ) ) ;
#22511 = DIRECTION ( 'NONE',  ( -0.000000000000000000, -1.000000000000000000, -0.000000000000000000 ) ) ;
#22512 = CARTESIAN_POINT ( 'NONE',  ( 0.3886748462736586696, 0.3298755754955758346, 0.06108448616840177897 ) ) ;
#22513 = CARTESIAN_POINT ( 'NONE',  ( 0.04625313968442696516, -0.5145616147176053090, 0.07046346805509963451 ) ) ;
#22514 = CIRCLE ( 'NONE', #12028, 0.01875000000000000625 ) ;
#22515 = CARTESIAN_POINT ( 'NONE',  ( 0.2764156081756483641, -0.1144950937579611028, 0.2793055555555589708 ) ) ;
#22516 = CARTESIAN_POINT ( 'NONE',  ( -0.2819296736111110979, 0.4659722221463555303, -3.452642723725051716E-17 ) ) ;
#22517 = CARTESIAN_POINT ( 'NONE',  ( 0.2764156081756483641, 0.1144950937579610056, -0.1026388888888885437 ) ) ;
#22518 = CARTESIAN_POINT ( 'NONE',  ( 0.1993543840281267465, 4.943138888964754507, 0.1993543840281266633 ) ) ;
#22519 = CARTESIAN_POINT ( 'NONE',  ( -0.3125000000000000000, 1.913510623667739771E-17, 0.3938888888888930628 ) ) ;
#22520 = CARTESIAN_POINT ( 'NONE',  ( -0.1167790944451423257, 4.842444444520309865, -0.2819296736111110424 ) ) ;
#22521 = CARTESIAN_POINT ( 'NONE',  ( -0.06335377612981447915, 0.08566948974967070196, 0.4000000000000000777 ) ) ;
#22522 = ADVANCED_FACE ( 'NONE', ( #16066, #17896 ), #6671, .F. ) ;
#22523 = LINE ( 'NONE', #2291, #5456 ) ;
#22524 = DIRECTION ( 'NONE',  ( -1.177540334020096294E-17, 0.2588190451025213501, -0.9659258262890680902 ) ) ;
#22525 = FACE_OUTER_BOUND ( 'NONE', #16036, .T. ) ;
#22526 = CARTESIAN_POINT ( 'NONE',  ( -0.1292346314604057023, 4.450083333333333613, 0.3119999999999998885 ) ) ;
#22527 = CARTESIAN_POINT ( 'NONE',  ( 0.1167790944451422702, 3.779944444520309865, -0.2819296736111110979 ) ) ;
#22528 = CARTESIAN_POINT ( 'NONE',  ( -0.2206173157302028232, 4.210499999999999687, -0.2206173157302028232 ) ) ;
#22529 = LINE ( 'NONE', #18754, #5773 ) ;
#22530 = FACE_OUTER_BOUND ( 'NONE', #12268, .T. ) ;
#22531 = VERTEX_POINT ( 'NONE', #3134 ) ;
#22532 = CARTESIAN_POINT ( 'NONE',  ( 0.3080688034448511026, 4.584097653652008830, 0.05047243502379121505 ) ) ;
#22533 = ORIENTED_EDGE ( 'NONE', *, *, #7391, .F. ) ;
#22534 = CC_DESIGN_PERSON_AND_ORGANIZATION_ASSIGNMENT ( #19900, #8796, ( #4895 ) ) ;
#22535 = ADVANCED_FACE ( 'NONE', ( #1188 ), #6034, .T. ) ;
#22536 = CARTESIAN_POINT ( 'NONE',  ( -0.1395639791202931690, -0.4606885764509979775, 0.4108348780186337201 ) ) ;
#22537 = VECTOR ( 'NONE', #20660, 39.37007874015748143 ) ;
#22538 = CARTESIAN_POINT ( 'NONE',  ( 0.2764557534944322437, 4.636758977684069194, 0.1492039665729707199 ) ) ;
#22539 =( BOUNDED_CURVE ( )  B_SPLINE_CURVE ( 2, ( #14104, #2762, #10213, #15923, #21532, #21416, #4705, #4820, #12173 ),
 .UNSPECIFIED., .F., .F. ) 
 B_SPLINE_CURVE_WITH_KNOTS ( ( 3, 2, 2, 2, 3 ),
 ( 0.6458333333333333703, 0.6562500000000000000, 0.6666666666666666297, 0.6770833333333333703, 0.6875000000000000000 ),
 .UNSPECIFIED. ) 
 CURVE ( )  GEOMETRIC_REPRESENTATION_ITEM ( )  RATIONAL_B_SPLINE_CURVE ( ( 1.000000000000000000, 0.9238795325112867385, 1.000000000000000000, 0.9238795325112867385, 1.000000000000000000, 0.9238795325112867385, 1.000000000000000000, 0.9238795325112867385, 1.000000000000000000 ) ) 
 REPRESENTATION_ITEM ( '' )  );
#22540 = CARTESIAN_POINT ( 'NONE',  ( -0.1954553509668046640, 0.1954553509668046918, 0.4147222222222267107 ) ) ;
#22541 = CARTESIAN_POINT ( 'NONE',  ( 0.4254318749130432953, 0.3089257318245579587, 0.05347049744907977215 ) ) ;
#22542 = CARTESIAN_POINT ( 'NONE',  ( -0.008932914564021687126, 3.932975559310150526, -0.3118903747639839574 ) ) ;
#22543 = CARTESIAN_POINT ( 'NONE',  ( 0.3028983722527614497, 5.146603643761612723, -0.01666118118391866215 ) ) ;
#22544 = ORIENTED_EDGE ( 'NONE', *, *, #6620, .F. ) ;
#22545 = CARTESIAN_POINT ( 'NONE',  ( 0.2233192592356399997, 0.2366071427596003751, -0.3073725909049500049 ) ) ;
#22546 = CARTESIAN_POINT ( 'NONE',  ( 0.2819296736111110424, 0.4208333332574666352, 0.1167790944451424923 ) ) ;
#22547 = CARTESIAN_POINT ( 'NONE',  ( -0.05830577631245405928, 5.206640035683668621, 0.2763456444142127766 ) ) ;
#22548 = CARTESIAN_POINT ( 'NONE',  ( 0.3043093620448166226, 0.5531817298998159549, -1.101755390420818603 ) ) ;
#22549 = CARTESIAN_POINT ( 'NONE',  ( 2.306251239869411052, 2.690142902515283208, -2.514111228547471377 ) ) ;
#22550 = CARTESIAN_POINT ( 'NONE',  ( -3.385114897866767815E-17, -0.2764156081756484196, 0.1091666666666686880 ) ) ;
#22551 = CARTESIAN_POINT ( 'NONE',  ( -0.3103109364157903838, 5.105077227193183909, -0.01115075287914376635 ) ) ;
#22552 = CARTESIAN_POINT ( 'NONE',  ( 0.4687500000000002776, -0.1744746749511749961, 0.4003434961619801169 ) ) ;
#22553 = CARTESIAN_POINT ( 'NONE',  ( 0.2206173157302027676, 0.1777777777777774515, 0.2206173157302028787 ) ) ;
#22554 = CARTESIAN_POINT ( 'NONE',  ( 0.2206173157302028787, 5.238277777777776478, 0.2206173157302027954 ) ) ;
#22555 = EDGE_CURVE ( 'NONE', #9589, #19562, #9226, .T. ) ;
#22556 = CARTESIAN_POINT ( 'NONE',  ( 0.1993543840281266633, 4.234805555631421470, -0.1993543840281266910 ) ) ;
#22557 = CARTESIAN_POINT ( 'NONE',  ( 9.101228903679513089E-16, 0.3732142855192008835, 0.4000000000000000222 ) ) ;
#22558 = B_SPLINE_CURVE_WITH_KNOTS ( 'NONE', 3,
 ( #6020, #13607, #19190, #9938, #11405, #20783, #4315, #4074, #18837, #18961, #7855, #17369, #9694, #15303, #660, #8087, #9452, #2133, #5670, #177, #13135, #11288, #18717, #2016, #7619, #13251, #22732, #15070, #22492, #8328, #4676, #4789, #10302, #21267, #6508, #23436, #12256, #21499, #6624 ),
 .UNSPECIFIED., .F., .F.,
 ( 4, 2, 2, 1, 2, 2, 1, 2, 2, 2, 2, 2, 2, 2, 2, 1, 2, 2, 2, 2, 4 ),
 ( 0.3563978319476573398, 0.3586778708967638396, 0.3609579098458703950, 0.3611004122801895200, 0.3611716634973491380, 0.3612072891059289192, 0.3612429147145087005, 0.3615279195831470060, 0.3620979293204236171, 0.3632379487949767838, 0.3643779682695300060, 0.3655179877440832281, 0.3666580072186363948, 0.3672280169559130059, 0.3675130218245513114, 0.3676555242588704364, 0.3677267754760300544, 0.3677980266931896169, 0.3700780656422960058, 0.3723581045914023391, 0.3746381435405087279 ),
 .UNSPECIFIED. ) ;
#22559 = VERTEX_POINT ( 'NONE', #17652 ) ;
#22560 = VERTEX_POINT ( 'NONE', #10586 ) ;
#22561 = CARTESIAN_POINT ( 'NONE',  ( -1.910449006669871087E-17, 4.314666666666665762, -0.3119999999999999996 ) ) ;
#22562 = CARTESIAN_POINT ( 'NONE',  ( 0.2819296736111110424, 4.939666666742532186, -0.1167790944451423396 ) ) ;
#22563 = ADVANCED_FACE ( 'NONE', ( #939 ), #23602, .T. ) ;
#22564 = CARTESIAN_POINT ( 'NONE',  ( -0.1985484582051802449, 5.148926605952134139, -0.2292351911855036173 ) ) ;
#22565 = DIRECTION ( 'NONE',  ( 0.5469441386039864961, -1.577721810442023611E-30, -0.8371691043312237124 ) ) ;
#22566 = DIRECTION ( 'NONE',  ( -0.000000000000000000, -1.000000000000000000, -0.000000000000000000 ) ) ;
#22567 = B_SPLINE_CURVE_WITH_KNOTS ( 'NONE', 3,
 ( #10603, #12688, #14753, #7184, #9250, #18275 ),
 .UNSPECIFIED., .F., .F.,
 ( 4, 2, 4 ),
 ( 5.421010862427522170E-20, 0.0002551367231383057919, 0.0005102734462766114754 ),
 .UNSPECIFIED. ) ;
#22568 = CARTESIAN_POINT ( 'NONE',  ( 0.1292346314604057300, 0.6118055554038226429, 0.3119999999999998885 ) ) ;
#22569 = VECTOR ( 'NONE', #6090, 39.37007874015748143 ) ;
#22570 = CARTESIAN_POINT ( 'NONE',  ( -0.2819296736111110979, 4.738277777853642903, -0.1167790944451422980 ) ) ;
#22571 = COORDINATED_UNIVERSAL_TIME_OFFSET ( 0, 0, .AHEAD. ) ;
#22572 = CARTESIAN_POINT ( 'NONE',  ( -0.04147181628195097114, 4.044975027077821750, -0.3093406118436980434 ) ) ;
#22573 = CARTESIAN_POINT ( 'NONE',  ( 0.2764156081756483641, -0.1144950937579611028, -0.04708333333333256099 ) ) ;
#22574 = CARTESIAN_POINT ( 'NONE',  ( -0.1993543840281266633, 0.5145833332574666352, -0.1993543840281266910 ) ) ;
#22575 = ORIENTED_EDGE ( 'NONE', *, *, #9829, .F. ) ;
#22576 = CARTESIAN_POINT ( 'NONE',  ( 0.1167790944451423535, 0.5388888888130222155, 0.2819296736111110424 ) ) ;
#22577 = CARTESIAN_POINT ( 'NONE',  ( 0.000000000000000000, 0.7650000000000000133, 0.000000000000000000 ) ) ;
#22578 = CARTESIAN_POINT ( 'NONE',  ( -0.06335377612981449302, 0.3393305098601595571, -0.4000000000000000222 ) ) ;
#22579 = CARTESIAN_POINT ( 'NONE',  ( -0.2472135954999579999, 0.1607142857142856429, 0.3402603233408159622 ) ) ;
#22580 = CARTESIAN_POINT ( 'NONE',  ( 0.1306872919485614071, -0.3155070326520293955, 0.1907638888888913420 ) ) ;
#22581 = CARTESIAN_POINT ( 'NONE',  ( 0.1294417382415921358, -0.3125000000000002220, 0.02930555555555713204 ) ) ;
#22582 = EDGE_CURVE ( 'NONE', #6423, #6354, #7776, .T. ) ;
#22583 = CARTESIAN_POINT ( 'NONE',  ( -0.2386280844053225714, -0.1440056533832719254, -0.06619720785293826959 ) ) ;
#22584 = CARTESIAN_POINT ( 'NONE',  ( -0.2819296736111110979, 0.3374999999241333759, -0.1167790944451423396 ) ) ;
#22585 = CARTESIAN_POINT ( 'NONE',  ( 0.2819296736111110979, 0.3131944443685777957, 0.000000000000000000 ) ) ;
#22586 = EDGE_CURVE ( 'NONE', #5967, #12731, #21141, .T. ) ;
#22587 = EDGE_CURVE ( 'NONE', #2181, #15406, #15789, .T. ) ;
#22588 = CARTESIAN_POINT ( 'NONE',  ( 0.2819296736111110979, 4.391055555631421470, 0.1167790944451422425 ) ) ;
#22589 = CARTESIAN_POINT ( 'NONE',  ( 0.4000000000000000222, 0.1767857140906294866, 0.000000000000000000 ) ) ;
#22590 = CARTESIAN_POINT ( 'NONE',  ( -0.1167790944451423535, 4.877166666742533963, 0.2819296736111110424 ) ) ;
#22591 = CARTESIAN_POINT ( 'NONE',  ( -0.1993543840281266355, 4.526472222298087544, 0.1993543840281267465 ) ) ;
#22592 = AXIS2_PLACEMENT_3D ( 'NONE', #5541, #15175, #9077 ) ;
#22593 = CYLINDRICAL_SURFACE ( 'NONE', #6733, 0.4000000000000000222 ) ;
#22594 = AXIS2_PLACEMENT_3D ( 'NONE', #12781, #1303, #18129 ) ;
#22595 = CARTESIAN_POINT ( 'NONE',  ( 5.731347020009612645E-17, 4.509111111111110404, 0.3119999999999999996 ) ) ;
#22596 = CARTESIAN_POINT ( 'NONE',  ( -0.3119999999999998885, 4.172305555707287894, 0.1292346314604058410 ) ) ;
#22597 = ADVANCED_FACE ( 'NONE', ( #5446 ), #5277, .T. ) ;
#22598 = CARTESIAN_POINT ( 'NONE',  ( -0.1236067977499789583, 0.2696428569477722914, -0.3804226065180614791 ) ) ;
#22599 = CARTESIAN_POINT ( 'NONE',  ( 0.000000000000000000, 5.384999999999999787, -0.3119999999999999996 ) ) ;
#22600 = ORIENTED_EDGE ( 'NONE', *, *, #6916, .F. ) ;
#22601 = SHAPE_DEFINITION_REPRESENTATION ( #14203, #1861 ) ;
#22602 = ORIENTED_EDGE ( 'NONE', *, *, #20625, .T. ) ;
#22603 = CARTESIAN_POINT ( 'NONE',  ( 0.2631830812676775877, 0.1021974198356748742, 0.3938365693361317033 ) ) ;
#22604 = AXIS2_PLACEMENT_3D ( 'NONE', #14359, #14119, #11951 ) ;
#22605 = CARTESIAN_POINT ( 'NONE',  ( -0.001863919267180048824, 3.514980167629567998, 2.816660016782450704 ) ) ;
#22606 = CARTESIAN_POINT ( 'NONE',  ( -0.2965161282126838049, 4.999381080173537661, -0.09725926298535028658 ) ) ;
#22607 = ORIENTED_EDGE ( 'NONE', *, *, #7206, .T. ) ;
#22608 = CARTESIAN_POINT ( 'NONE',  ( 0.2206173157302028232, 0.4624999998482670627, -0.2206173157302028232 ) ) ;
#22609 = CIRCLE ( 'NONE', #16009, 0.3125000000000001665 ) ;
#22610 = ORIENTED_EDGE ( 'NONE', *, *, #7888, .F. ) ;
#22611 = DIRECTION ( 'NONE',  ( -0.4999999999999909517, 0.000000000000000000, 0.8660254037844438146 ) ) ;
#22612 = LINE ( 'NONE', #13355, #7330 ) ;
#22613 = CARTESIAN_POINT ( 'NONE',  ( 0.04740204007499370514, 4.764705480950462757, -0.3086056850508328009 ) ) ;
#22614 = CARTESIAN_POINT ( 'NONE',  ( -0.2923287055106771337, 0.03660714275960045422, 0.2123892367102619971 ) ) ;
#22615 = CYLINDRICAL_SURFACE ( 'NONE', #341, 0.4062499999999997780 ) ;
#22616 = ORIENTED_EDGE ( 'NONE', *, *, #4975, .F. ) ;
#22617 = CARTESIAN_POINT ( 'NONE',  ( -0.2233192592356400275, 0.3437499999024575259, 0.3073725909049499494 ) ) ;
#22618 = ORIENTED_EDGE ( 'NONE', *, *, #6146, .F. ) ;
#22619 = CARTESIAN_POINT ( 'NONE',  ( 3.820898013339742174E-17, 5.384999999999999787, 0.3119999999999999996 ) ) ;
#22620 = CARTESIAN_POINT ( 'NONE',  ( -0.1144950937579609779, 0.2764156081756484196, 0.4112500000000044453 ) ) ;
#22621 = CARTESIAN_POINT ( 'NONE',  ( 0.2819296736111110424, 4.106333333409199149, -0.1167790944451423396 ) ) ;
#22622 = CARTESIAN_POINT ( 'NONE',  ( 0.000000000000000000, 3.700000000000000622, -0.4000000000000000222 ) ) ;
#22623 = CARTESIAN_POINT ( 'NONE',  ( -0.2206173157302028232, 4.821611111111110404, -0.2206173157302028232 ) ) ;
#22624 = CARTESIAN_POINT ( 'NONE',  ( -0.2206173157302028232, 3.766055555555554601, -0.2206173157302028232 ) ) ;
#22625 = CARTESIAN_POINT ( 'NONE',  ( 0.3119999999999999996, 4.700083333485065573, -0.1292346314604056745 ) ) ;
#22626 = EDGE_CURVE ( 'NONE', #8318, #1635, #2917, .T. ) ;
#22627 = CARTESIAN_POINT ( 'NONE',  ( 0.1993543840281266633, 5.012583333409199149, -0.1993543840281266910 ) ) ;
#22628 = ORIENTED_EDGE ( 'NONE', *, *, #8915, .F. ) ;
#22629 = CARTESIAN_POINT ( 'NONE',  ( -0.1993543840281266910, 4.290361111186976828, -0.1993543840281266910 ) ) ;
#22630 = ORIENTED_EDGE ( 'NONE', *, *, #8536, .F. ) ;
#22631 = CARTESIAN_POINT ( 'NONE',  ( -0.2233192592356400275, 0.1830357141881718552, 0.3073725909049499494 ) ) ;
#22632 = EDGE_LOOP ( 'NONE', ( #18825, #14336, #4321, #9803, #13905, #14713 ) ) ;
#22633 = ORIENTED_EDGE ( 'NONE', *, *, #23018, .T. ) ;
#22634 = DATE_TIME_ROLE ( 'classification_date' ) ;
#22635 = CARTESIAN_POINT ( 'NONE',  ( 0.1306872919485616846, 0.3155070326520292290, 0.4372916666666715191 ) ) ;
#22636 = DIRECTION ( 'NONE',  ( -0.000000000000000000, 1.000000000000000000, -0.000000000000000000 ) ) ;
#22637 = CARTESIAN_POINT ( 'NONE',  ( 0.1167790944451422702, 3.960500000075866112, -0.2819296736111110979 ) ) ;
#22638 = DIRECTION ( 'NONE',  ( -0.8660254037844434816, 0.000000000000000000, -0.4999999999999915068 ) ) ;
#22639 = CARTESIAN_POINT ( 'NONE',  ( 0.1144950937579609085, -0.2764156081756484751, 0.3348611111111149397 ) ) ;
#22640 = CARTESIAN_POINT ( 'NONE',  ( 7.256325792998745354E-13, 0.06073895945496885634, 0.3102389594549692098 ) ) ;
#22641 = CARTESIAN_POINT ( 'NONE',  ( 0.000000000000000000, 0.2764156081756484196, 0.3522222222222262111 ) ) ;
#22642 = CARTESIAN_POINT ( 'NONE',  ( -0.1167790944451422702, 0.4555555554796890116, -0.2819296736111110979 ) ) ;
#22643 = CARTESIAN_POINT ( 'NONE',  ( -0.1954553509668046640, 0.1954553509668046918, -0.08527777777777728607 ) ) ;
#22644 = CARTESIAN_POINT ( 'NONE',  ( -0.2819296736111110424, 4.974388888964754507, -0.1167790944451423119 ) ) ;
#22645 = CARTESIAN_POINT ( 'NONE',  ( -0.2206173157302028232, 3.932722222222221120, -0.2206173157302028232 ) ) ;
#22646 = CARTESIAN_POINT ( 'NONE',  ( -1.726321361862525858E-17, 4.561194444520309865, -0.2819296736111110979 ) ) ;
#22647 = CARTESIAN_POINT ( 'NONE',  ( -0.2525416622817135415, 0.1285646679930061709, -0.07191566027702570030 ) ) ;
#22648 = CARTESIAN_POINT ( 'NONE',  ( 0.2893869579258043223, 4.866662948179751425, -0.1166288015440531262 ) ) ;
#22649 = FACE_OUTER_BOUND ( 'NONE', #13721, .T. ) ;
#22650 = CARTESIAN_POINT ( 'NONE',  ( 0.2798077087188375889, -0.01523944824432932332, 0.3914743753855044472 ) ) ;
#22651 = CARTESIAN_POINT ( 'NONE',  ( 0.1292346314604056190, 4.533416666666664874, -0.3119999999999999996 ) ) ;
#22652 = CARTESIAN_POINT ( 'NONE',  ( 0.2819296736111110979, 3.884111111186976384, -0.1167790944451423396 ) ) ;
#22653 = CARTESIAN_POINT ( 'NONE',  ( -0.3119999999999998885, 4.220916666666665762, 0.1292346314604058410 ) ) ;
#22654 = CARTESIAN_POINT ( 'NONE',  ( -0.3119999999999999996, 0.5354166665149336923, -0.1292346314604056745 ) ) ;
#22655 = VERTEX_POINT ( 'NONE', #8862 ) ;
#22656 = CARTESIAN_POINT ( 'NONE',  ( 0.2487385569593157653, 4.591261249557366142, -0.1929159009956799564 ) ) ;
#22657 = EDGE_LOOP ( 'NONE', ( #23947, #2445, #10104, #22020 ) ) ;
#22658 = CARTESIAN_POINT ( 'NONE',  ( -0.1735004431958599436, 4.121918744418447744, 0.2593098876758328508 ) ) ;
#22659 = FACE_OUTER_BOUND ( 'NONE', #4395, .T. ) ;
#22660 = CARTESIAN_POINT ( 'NONE',  ( 0.000000000000000000, 0.2764156081756484196, 0.3522222222222262111 ) ) ;
#22661 = CARTESIAN_POINT ( 'NONE',  ( -0.1917384371582980807, 3.938511949306523707, -0.2494961635661361310 ) ) ;
#22662 = ORIENTED_EDGE ( 'NONE', *, *, #22270, .T. ) ;
#22663 = CARTESIAN_POINT ( 'NONE',  ( 0.1116596296178199860, 0.008035714188171883682, -0.3436530038418508792 ) ) ;
#22664 = CARTESIAN_POINT ( 'NONE',  ( -0.2819296736111110979, 0.4555555554796890116, 0.1167790944451422425 ) ) ;
#22665 = CARTESIAN_POINT ( 'NONE',  ( -0.07707608760941696280, 5.206640035683669510, 0.2713641110486283980 ) ) ;
#22666 = CARTESIAN_POINT ( 'NONE',  ( -1.322549964794167179E-16, 0.7885332705621128646, -1.079944001585411595 ) ) ;
#22667 = CARTESIAN_POINT ( 'NONE',  ( 2.952666666666668327, 2.723333333333333606, -0.03333333333333364512 ) ) ;
#22668 = CARTESIAN_POINT ( 'NONE',  ( 0.2764156081756484196, -5.077672346800151106E-17, 0.1230555555555576941 ) ) ;
#22669 = CARTESIAN_POINT ( 'NONE',  ( -0.3111413042013332908, 4.614172690785681930, 0.03290619045792032848 ) ) ;
#22670 = DIRECTION ( 'NONE',  ( -0.4999999999999931166, -6.654928120984804281E-16, -0.8660254037844425934 ) ) ;
#22671 = CARTESIAN_POINT ( 'NONE',  ( -0.3119999999999999996, 0.2680555555555552139, -3.820898013339742174E-17 ) ) ;
#22672 = CARTESIAN_POINT ( 'NONE',  ( -0.2206173157302028232, 5.210499999999999687, -0.2206173157302028232 ) ) ;
#22673 = CARTESIAN_POINT ( 'NONE',  ( 0.2819296736111110424, 4.286888888964754507, -0.1167790944451423396 ) ) ;
#22674 = CARTESIAN_POINT ( 'NONE',  ( -0.03750733961385160214, 0.5077191469176455252, 0.4064695056028757580 ) ) ;
#22675 = CARTESIAN_POINT ( 'NONE',  ( 0.3999999999999999667, 0.3874999998049150629, 0.1299678784931626307 ) ) ;
#22676 = ORIENTED_EDGE ( 'NONE', *, *, #18817, .T. ) ;
#22677 = ORIENTED_EDGE ( 'NONE', *, *, #14198, .F. ) ;
#22678 = CARTESIAN_POINT ( 'NONE',  ( 0.3119999999999998885, 0.3479166666666662633, 0.1292346314604058410 ) ) ;
#22679 = CARTESIAN_POINT ( 'NONE',  ( -0.1993543840281266355, 4.693138888964754507, 0.1993543840281267465 ) ) ;
#22680 = CIRCLE ( 'NONE', #487, 0.01875000000000000625 ) ;
#22681 =( BOUNDED_CURVE ( )  B_SPLINE_CURVE ( 2, ( #21304, #4597, #12055 ),
 .UNSPECIFIED., .F., .F. ) 
 B_SPLINE_CURVE_WITH_KNOTS ( ( 3, 3 ),
 ( 1.734723475976807094E-18, 0.002646478566469958466 ),
 .UNSPECIFIED. ) 
 CURVE ( )  GEOMETRIC_REPRESENTATION_ITEM ( )  RATIONAL_B_SPLINE_CURVE ( ( 1.000000000000000000, 0.4999999999999997780, 1.000000000000000000 ) ) 
 REPRESENTATION_ITEM ( '' )  );
#22682 = CARTESIAN_POINT ( 'NONE',  ( -0.07811407312994299301, 5.145356041543204029, -0.2939319536219872631 ) ) ;
#22683 = CARTESIAN_POINT ( 'NONE',  ( 0.5116234456863258950, -1.819812086079792390, 2.202095583405667689 ) ) ;
#22684 = CARTESIAN_POINT ( 'NONE',  ( 0.0002793920057309124327, 3.710492493090175259, -0.3119999064896394336 ) ) ;
#22685 = CARTESIAN_POINT ( 'NONE',  ( 0.2764156081756483641, 0.1144950937579610056, -0.1026388888888885437 ) ) ;
#22686 = CARTESIAN_POINT ( 'NONE',  ( 5.178964085587577574E-17, 4.325083333409199149, 0.2819296736111110979 ) ) ;
#22688 = EDGE_CURVE ( 'NONE', #22475, #5943, #8730, .T. ) ;
#22687 = APPROVAL_DATE_TIME ( #493, #23253 ) ;
#22689 = CARTESIAN_POINT ( 'NONE',  ( -0.03372224778004788426, 4.044757933730085853, -0.3102599952880983336 ) ) ;
#22690 = CARTESIAN_POINT ( 'NONE',  ( 0.000000000000000000, 0.2764156081756484196, 0.08138888888889070361 ) ) ;
#22691 = DIRECTION ( 'NONE',  ( 1.000000000000000000, 0.000000000000000000, 1.224646799147353207E-16 ) ) ;
#22692 = CARTESIAN_POINT ( 'NONE',  ( 1.726321361862525858E-17, 0.5631944443685776847, -0.2819296736111110979 ) ) ;
#22693 = SPHERICAL_SURFACE ( 'NONE', #3773, 0.7650000000000000133 ) ;
#22694 = LINE ( 'NONE', #7933, #15995 ) ;
#22695 = CARTESIAN_POINT ( 'NONE',  ( -0.2472135954999579444, 0.1392857142857142350, -0.3402603233408159622 ) ) ;
#22696 = CARTESIAN_POINT ( 'NONE',  ( 0.1306872919485616846, 0.3155070326520292290, 0.1004861111111128580 ) ) ;
#22697 = EDGE_CURVE ( 'NONE', #23979, #16523, #9231, .T. ) ;
#22698 = LINE ( 'NONE', #18801, #5978 ) ;
#22699 = CARTESIAN_POINT ( 'NONE',  ( -0.2533266501256048464, -0.1176800686429169962, -0.06681963058184084425 ) ) ;
#22700 = CARTESIAN_POINT ( 'NONE',  ( -0.1167790944451422702, 0.4416666665908000611, -0.2819296736111110979 ) ) ;
#22701 = CARTESIAN_POINT ( 'NONE',  ( -0.1993543840281266633, 0.3340277777019111660, -0.1993543840281266910 ) ) ;
#22702 = CARTESIAN_POINT ( 'NONE',  ( -0.1167790944451423535, 4.266055555631421470, 0.2819296736111110424 ) ) ;
#22703 = CARTESIAN_POINT ( 'NONE',  ( -0.2472135954999579444, 0.3446428569477723025, -0.3402603233408159622 ) ) ;
#22704 = CARTESIAN_POINT ( 'NONE',  ( -0.1993543840281266355, 4.873694444520310753, 0.1993543840281267465 ) ) ;
#22705 = CARTESIAN_POINT ( 'NONE',  ( 0.1993543840281267465, 4.318138888964754507, 0.1993543840281266633 ) ) ;
#22706 = FACE_OUTER_BOUND ( 'NONE', #10129, .T. ) ;
#22707 = ORIENTED_EDGE ( 'NONE', *, *, #20816, .F. ) ;
#22708 = PLANE ( 'NONE',  #15951 ) ;
#22709 = CARTESIAN_POINT ( 'NONE',  ( -0.3119999999999998885, 4.005638889040620931, 0.1292346314604058410 ) ) ;
#22710 = CARTESIAN_POINT ( 'NONE',  ( 0.1292346314604057300, 0.1187499999999996614, 0.3119999999999998885 ) ) ;
#22711 = CARTESIAN_POINT ( 'NONE',  ( 0.2552321839962294336, -0.1601952157746480421, -0.09003777342340114898 ) ) ;
#22712 = ORIENTED_EDGE ( 'NONE', *, *, #6893, .F. ) ;
#22713 = EDGE_CURVE ( 'NONE', #21880, #20052, #1908, .T. ) ;
#22714 = EDGE_CURVE ( 'NONE', #15814, #20917, #18980, .T. ) ;
#22715 = PERSON_AND_ORGANIZATION_ROLE ( 'design_owner' ) ;
#22716 = DIRECTION ( 'NONE',  ( 0.000000000000000000, 0.000000000000000000, 1.000000000000000000 ) ) ;
#22717 = CARTESIAN_POINT ( 'NONE',  ( -0.02214754980521025859, 4.848813742978035357, 0.3119999961461823457 ) ) ;
#22718 = CARTESIAN_POINT ( 'NONE',  ( -0.2884719277531277437, 4.998711128422118399, -0.1188678792519748117 ) ) ;
#22719 = VERTEX_POINT ( 'NONE', #11551 ) ;
#22720 = CARTESIAN_POINT ( 'NONE',  ( 0.3119999999999999996, 0.5145833331816003220, -0.1292346314604056468 ) ) ;
#22721 = EDGE_LOOP ( 'NONE', ( #5427, #2475, #16086, #10400 ) ) ;
#22722 = CARTESIAN_POINT ( 'NONE',  ( 0.07773895667863905956, 4.263908277548741133, -0.3027182936550676384 ) ) ;
#22723 = CARTESIAN_POINT ( 'NONE',  ( -0.1292346314604068958, 4.651472222222221120, -0.3119999999999987228 ) ) ;
#22724 = CARTESIAN_POINT ( 'NONE',  ( 0.000000000000000000, 3.738758431839877614E-19, 0.004799741732707325965 ) ) ;
#22725 = CARTESIAN_POINT ( 'NONE',  ( 0.1116596296178199860, 0.07946428561674331870, -0.3436530038418508792 ) ) ;
#22726 = CARTESIAN_POINT ( 'NONE',  ( 0.2543668527069268270, 5.175014549981658440, 0.1503412913315801680 ) ) ;
#22727 = ADVANCED_FACE ( 'NONE', ( #11306 ), #9959, .T. ) ;
#22728 =( BOUNDED_CURVE ( )  B_SPLINE_CURVE ( 2, ( #23110, #14224, #15810, #8360, #6419, #21536, #1178, #6783, #8125 ),
 .UNSPECIFIED., .F., .T. ) 
 B_SPLINE_CURVE_WITH_KNOTS ( ( 3, 2, 2, 2, 3 ),
 ( 0.3958333333333334259, 0.4062500000000001110, 0.4166666666666667407, 0.4270833333333333703, 0.4375000000000000555 ),
 .UNSPECIFIED. ) 
 CURVE ( )  GEOMETRIC_REPRESENTATION_ITEM ( )  RATIONAL_B_SPLINE_CURVE ( ( 0.9999999999999992228, 0.9238795325112875156, 1.000000000000000000, 0.9238795325112867385, 1.000000000000000000, 0.9238795325112867385, 1.000000000000000000, 0.9238795325112862944, 1.000000000000000444 ) ) 
 REPRESENTATION_ITEM ( '' )  );
#22729 = ORIENTED_EDGE ( 'NONE', *, *, #22442, .T. ) ;
#22730 = CARTESIAN_POINT ( 'NONE',  ( 0.3613381517857143232, 0.4366071427596003862, 0.1174058825155741975 ) ) ;
#22731 = DIRECTION ( 'NONE',  ( 0.4999999999999919509, 0.000000000000000000, 0.8660254037844431485 ) ) ;
#22732 = CARTESIAN_POINT ( 'NONE',  ( -0.2965167191063861618, 4.666047801639679804, -0.09725748803006217802 ) ) ;
#22733 = CIRCLE ( 'NONE', #21560, 0.2041999999999999926 ) ;
#22734 = CARTESIAN_POINT ( 'NONE',  ( 0.1993543840281266633, 3.998694444520309865, -0.1993543840281266910 ) ) ;
#22735 = FACE_OUTER_BOUND ( 'NONE', #13598, .T. ) ;
#22736 = DIRECTION ( 'NONE',  ( -0.8459207832372979130, 0.4883925919151543282, -0.2142211582677917836 ) ) ;
#22737 = CARTESIAN_POINT ( 'NONE',  ( -0.2144645408843714462, 5.188090166419283555, 0.1954364597099001455 ) ) ;
#22738 = CARTESIAN_POINT ( 'NONE',  ( 0.1292346314604056190, 4.651472222373953969, -0.3119999999999999996 ) ) ;
#22739 = CARTESIAN_POINT ( 'NONE',  ( -0.2819296736111110979, 4.974388888964754507, -0.1167790944451422980 ) ) ;
#22740 = ORIENTED_EDGE ( 'NONE', *, *, #5216, .T. ) ;
#22741 = ADVANCED_FACE ( 'NONE', ( #17151 ), #19093, .T. ) ;
#22742 = CARTESIAN_POINT ( 'NONE',  ( 0.1167790944451424368, 4.259111111186975940, 0.2819296736111110424 ) ) ;
#22743 = ORIENTED_EDGE ( 'NONE', *, *, #13083, .F. ) ;
#22744 = CARTESIAN_POINT ( 'NONE',  ( 0.1116596296178199027, 0.1223214284738861762, 0.3436530038418508792 ) ) ;
#22745 = ORIENTED_EDGE ( 'NONE', *, *, #12285, .T. ) ;
#22746 = ORIENTED_EDGE ( 'NONE', *, *, #9881, .T. ) ;
#22747 = APPROVAL_DATE_TIME ( #22865, #15224 ) ;
#22748 = CIRCLE ( 'NONE', #4448, 0.2500000000000000555 ) ;
#22749 = DIRECTION ( 'NONE',  ( 1.000000000000000000, 0.000000000000000000, 0.000000000000000000 ) ) ;
#22750 = CARTESIAN_POINT ( 'NONE',  ( 1.573500000000000343, 2.740000000000000213, -1.412500000000000089 ) ) ;
#22751 = CARTESIAN_POINT ( 'NONE',  ( 0.2819296736111111534, 3.891055555631421470, 0.1167790944451422563 ) ) ;
#22752 = CARTESIAN_POINT ( 'NONE',  ( 0.1000962206091226825, 4.429843089621714469, -0.2955515137184793195 ) ) ;
#22753 = CARTESIAN_POINT ( 'NONE',  ( 0.3120000000000000551, 4.630638888888888083, 0.1292346314604056190 ) ) ;
#22754 = CARTESIAN_POINT ( 'NONE',  ( 0.06525658555531335669, 0.06189869434473758980, 0.3049238613443945312 ) ) ;
#22755 = CARTESIAN_POINT ( 'NONE',  ( 0.2764156081756483641, -0.1144950937579611028, 0.1681944444444470055 ) ) ;
#22756 = CARTESIAN_POINT ( 'NONE',  ( 0.1167790944451423119, 0.4486111110352445364, -0.2819296736111110979 ) ) ;
#22757 = CARTESIAN_POINT ( 'NONE',  ( 0.1954553509668046640, -0.1954553509668047195, 0.3938888888888931739 ) ) ;
#22758 = EDGE_LOOP ( 'NONE', ( #7014, #21611, #11545, #18198 ) ) ;
#22759 = CARTESIAN_POINT ( 'NONE',  ( 0.1167790944451424368, 4.828555555631421470, 0.2819296736111110424 ) ) ;
#22760 = FACE_OUTER_BOUND ( 'NONE', #23353, .T. ) ;
#22761 = CARTESIAN_POINT ( 'NONE',  ( 0.2819296736111110424, 4.773000000075865223, -0.1167790944451423396 ) ) ;
#22762 = CARTESIAN_POINT ( 'NONE',  ( -0.1209188320989881132, 0.2598538660581654614, -0.07562110105720883102 ) ) ;
#22763 = CARTESIAN_POINT ( 'NONE',  ( 7.256325792998745354E-13, 0.06073895945496885634, 0.3102389594549692098 ) ) ;
#22764 = LINE ( 'NONE', #21057, #1275 ) ;
#22765 = CARTESIAN_POINT ( 'NONE',  ( 0.2782766723721453728, -0.03026958819840001175, 0.3911785983335306360 ) ) ;
#22766 = CARTESIAN_POINT ( 'NONE',  ( -0.2206173157302028232, 4.599388888888888083, -0.2206173157302028232 ) ) ;
#22767 = CARTESIAN_POINT ( 'NONE',  ( 0.2819296736111110979, 3.880638888964754063, -3.452642723725051716E-17 ) ) ;
#22768 = CARTESIAN_POINT ( 'NONE',  ( 0.0003180184531269840040, 4.988268656965369807, -0.3120000001075144969 ) ) ;
#22769 = ORIENTED_EDGE ( 'NONE', *, *, #1453, .F. ) ;
#22770 = CARTESIAN_POINT ( 'NONE',  ( 2.100416254512341485, 2.978485840173427324, -2.201288568297000925 ) ) ;
#22771 = ORIENTED_EDGE ( 'NONE', *, *, #7092, .T. ) ;
#22772 = CC_DESIGN_APPROVAL ( #8045, ( #7598 ) ) ;
#22773 = CARTESIAN_POINT ( 'NONE',  ( 0.3086474089601525805, 4.639775044814750338, 0.04641666148907084427 ) ) ;
#22774 = CARTESIAN_POINT ( 'NONE',  ( -0.3155070326520292845, 1.931923388228935888E-17, -0.1564583333333331994 ) ) ;
#22775 = EDGE_CURVE ( 'NONE', #8952, #5177, #5099, .T. ) ;
#22776 = VECTOR ( 'NONE', #16874, 39.37007874015748143 ) ;
#22777 = CARTESIAN_POINT ( 'NONE',  ( -0.01786144021398791693, 3.933228899117950927, -0.3115615334367522471 ) ) ;
#22778 = EDGE_CURVE ( 'NONE', #5409, #1715, #2034, .T. ) ;
#22779 = ORIENTED_EDGE ( 'NONE', *, *, #17219, .T. ) ;
#22780 = CARTESIAN_POINT ( 'NONE',  ( -0.2233192592356399997, 0.4151785713310289783, 0.3073725909049499494 ) ) ;
#22781 = CARTESIAN_POINT ( 'NONE',  ( -0.2819296736111110424, 0.3930555554796889561, -0.1167790944451423396 ) ) ;
#22782 = CARTESIAN_POINT ( 'NONE',  ( -3.385114897866767815E-17, -0.2764156081756484196, -0.1130555555555552844 ) ) ;
#22783 = DIRECTION ( 'NONE',  ( 0.000000000000000000, 1.000000000000000000, 0.000000000000000000 ) ) ;
#22784 = CARTESIAN_POINT ( 'NONE',  ( 0.3119999999999999996, 0.5180555555555551583, 0.000000000000000000 ) ) ;
#22785 = CARTESIAN_POINT ( 'NONE',  ( 0.1954553509668047195, 0.1954553509668046085, 0.2411111111111141903 ) ) ;
#22786 = CARTESIAN_POINT ( 'NONE',  ( -0.04069169679679301294, 5.117267119184975677, 0.3063199299893399896 ) ) ;
#22787 = CARTESIAN_POINT ( 'NONE',  ( 0.2472135954999579721, 0.1160714283763437660, -0.3402603233408160732 ) ) ;
#22788 = CC_DESIGN_APPROVAL ( #13438, ( #13174 ) ) ;
#22789 = CARTESIAN_POINT ( 'NONE',  ( 0.2206173157302028787, 4.738277777777777366, 0.2206173157302027954 ) ) ;
#22790 = CARTESIAN_POINT ( 'NONE',  ( 0.3119999999999999996, 0.1881944444444441089, -0.1292346314604056468 ) ) ;
#22791 = CARTESIAN_POINT ( 'NONE',  ( -0.3119999999999999996, 5.102861111111111292, -0.1292346314604056468 ) ) ;
#22792 = CARTESIAN_POINT ( 'NONE',  ( 0.1167790944451424368, 4.273000000075865223, 0.2819296736111110424 ) ) ;
#22793 = CARTESIAN_POINT ( 'NONE',  ( -0.3039181560427893225, 4.333230708440404477, -0.08152835368557848073 ) ) ;
#22794 = CARTESIAN_POINT ( 'NONE',  ( 0.000000000000000000, 3.700000000000000622, 0.000000000000000000 ) ) ;
#22795 = CARTESIAN_POINT ( 'NONE',  ( 8.817456953860933428E-17, 3.700000000000000622, 0.7199999999999994182 ) ) ;
#22796 = ORIENTED_EDGE ( 'NONE', *, *, #3497, .F. ) ;
#22797 = CARTESIAN_POINT ( 'NONE',  ( -0.1060554323913586589, 3.066692553488282957, 2.783525011231007706 ) ) ;
#22798 = CARTESIAN_POINT ( 'NONE',  ( -0.1993543840281266910, 4.679250000075866112, -0.1993543840281266910 ) ) ;
#22799 = AXIS2_PLACEMENT_3D ( 'NONE', #53, #16415, #7145 ) ;
#22800 = CARTESIAN_POINT ( 'NONE',  ( 0.2233192592356399164, 0.4116071427596004195, 0.3073725909049500604 ) ) ;
#22801 = CARTESIAN_POINT ( 'NONE',  ( 1.124754269082862912, 2.291712385858714285, -0.4073223533918538530 ) ) ;
#22802 = APPROVAL_STATUS ( 'not_yet_approved' ) ;
#22803 = CARTESIAN_POINT ( 'NONE',  ( -8.964115882027956832E-07, 3.710500024236165206, -0.3119999999987121964 ) ) ;
#22804 = APPROVAL ( #20768, 'UNSPECIFIED' ) ;
#22805 = CARTESIAN_POINT ( 'NONE',  ( 0.1144950937579611444, 0.2764156081756483641, -0.09569444444444404063 ) ) ;
#22806 = CC_DESIGN_SECURITY_CLASSIFICATION ( #19708, ( #24132 ) ) ;
#22807 = CARTESIAN_POINT ( 'NONE',  ( 0.1993543840281266633, 4.345916666742532186, -0.1993543840281266910 ) ) ;
#22808 = COORDINATED_UNIVERSAL_TIME_OFFSET ( 0, 0, .AHEAD. ) ;
#22809 = CARTESIAN_POINT ( 'NONE',  ( -0.2629549181022274862, 4.062781045653800938, 0.1724798338529683339 ) ) ;
#22810 = CARTESIAN_POINT ( 'NONE',  ( 0.1954553509668046640, -0.1954553509668047195, 0.06055555555555720143 ) ) ;
#22811 = FACE_OUTER_BOUND ( 'NONE', #2678, .T. ) ;
#22812 = EDGE_LOOP ( 'NONE', ( #7866, #18975, #14288, #5485 ) ) ;
#22813 = CARTESIAN_POINT ( 'NONE',  ( -0.2819296736111110424, 0.5180555554796888451, -0.1167790944451423396 ) ) ;
#22814 = LINE ( 'NONE', #6104, #20139 ) ;
#22815 = CARTESIAN_POINT ( 'NONE',  ( 0.2209708691207961095, -0.2209708691207961651, 0.1925000000000024747 ) ) ;
#22816 = CARTESIAN_POINT ( 'NONE',  ( 0.3236067977499789694, 0.1071428571428571092, 0.2351141009169893659 ) ) ;
#22817 = CARTESIAN_POINT ( 'NONE',  ( -0.1306872919485614903, 0.3155070326520293400, 0.1629861111111133576 ) ) ;
#22818 = CARTESIAN_POINT ( 'NONE',  ( 0.3124999999999991673, 0.1294417382415931073, 0.03625000000000128814 ) ) ;
#22819 = FACE_OUTER_BOUND ( 'NONE', #17020, .T. ) ;
#22820 = CARTESIAN_POINT ( 'NONE',  ( 0.2819296736111110979, 0.5944444443685777957, -0.1167790944451422980 ) ) ;
#22821 = CARTESIAN_POINT ( 'NONE',  ( -0.1167790944451422702, 0.1638888888130222432, -0.2819296736111110424 ) ) ;
#22822 = CARTESIAN_POINT ( 'NONE',  ( -0.1993543840281266355, 4.318138888964754507, 0.1993543840281267465 ) ) ;
#22823 = CARTESIAN_POINT ( 'NONE',  ( -0.4000000000000000222, 0.2839285712334865819, -4.898587196589413075E-17 ) ) ;
#22824 = CARTESIAN_POINT ( 'NONE',  ( 0.1167790944451424368, 4.884111111186977716, 0.2819296736111110424 ) ) ;
#22825 =( BOUNDED_CURVE ( )  B_SPLINE_CURVE ( 2, ( #1081, #6448, #15838, #19493, #1207, #19734, #12559, #17550, #19613 ),
 .UNSPECIFIED., .F., .F. ) 
 B_SPLINE_CURVE_WITH_KNOTS ( ( 3, 2, 2, 2, 3 ),
 ( 0.8541666666666666297, 0.8645833333333333703, 0.8750000000000000000, 0.8854166666666666297, 0.8958333333333333703 ),
 .UNSPECIFIED. ) 
 CURVE ( )  GEOMETRIC_REPRESENTATION_ITEM ( )  RATIONAL_B_SPLINE_CURVE ( ( 1.000000000000000000, 0.9238795325112867385, 1.000000000000000000, 0.9238795325112867385, 1.000000000000000000, 0.9238795325112867385, 1.000000000000000000, 0.9238795325112867385, 1.000000000000000000 ) ) 
 REPRESENTATION_ITEM ( '' )  );
#22826 = CARTESIAN_POINT ( 'NONE',  ( 0.1167790944451422702, 4.335500000075866112, -0.2819296736111110979 ) ) ;
#22827 = EDGE_CURVE ( 'NONE', #1154, #12827, #20686, .T. ) ;
#22828 = LINE ( 'NONE', #11626, #10638 ) ;
#22829 = ORIENTED_EDGE ( 'NONE', *, *, #1557, .T. ) ;
#22830 = CARTESIAN_POINT ( 'NONE',  ( 0.7847114317029993957, 2.291712385858714285, -0.8254988538245819907 ) ) ;
#22831 = CARTESIAN_POINT ( 'NONE',  ( 0.3119999999999999996, 3.866750000151731648, -0.1292346314604056745 ) ) ;
#22832 = CARTESIAN_POINT ( 'NONE',  ( 0.000000000000000000, 0.1799999999999999933, 1.243000000000000105 ) ) ;
#22833 = AXIS2_PLACEMENT_3D ( 'NONE', #23430, #23309, #6986 ) ;
#22834 = EDGE_CURVE ( 'NONE', #397, #21142, #9594, .T. ) ;
#22835 = CARTESIAN_POINT ( 'NONE',  ( -0.06232504193995545838, -0.3017193634690832349, -0.09679842907668260998 ) ) ;
#22836 = ORIENTED_EDGE ( 'NONE', *, *, #9659, .F. ) ;
#22837 = PERSON_AND_ORGANIZATION ( #15518, #2538 ) ;
#22838 = CARTESIAN_POINT ( 'NONE',  ( 5.574357792518489764E-07, 4.071633398088104094, 0.3119999999989289674 ) ) ;
#22839 = CARTESIAN_POINT ( 'NONE',  ( -0.5116234456863258950, 1.658283848634127366, -2.640781157734872320 ) ) ;
#22840 = EDGE_LOOP ( 'NONE', ( #5122, #12674, #21664, #18069 ) ) ;
#22841 = CARTESIAN_POINT ( 'NONE',  ( -0.1993543840281266633, 0.1256944443685777957, -0.1993543840281266910 ) ) ;
#22842 = ORIENTED_EDGE ( 'NONE', *, *, #17863, .T. ) ;
#22843 = CARTESIAN_POINT ( 'NONE',  ( 0.001519364365302375416, 4.266014716456939304, -0.3119968335204331700 ) ) ;
#22844 = CARTESIAN_POINT ( 'NONE',  ( 0.2139474665362423589, 0.4177432499681213995, 0.4289390872834607515 ) ) ;
#22845 = CARTESIAN_POINT ( 'NONE',  ( 0.2897599955979855979, 4.755713818965608297, -0.1232763402910086042 ) ) ;
#22846 = CARTESIAN_POINT ( 'NONE',  ( 0.2233192592356399997, 0.07589285704531473220, -0.3073725909049500049 ) ) ;
#22847 = CARTESIAN_POINT ( 'NONE',  ( 0.2209006037727569149, 5.173586066099031378, 0.1969744680321389718 ) ) ;
#22848 = VERTEX_POINT ( 'NONE', #1164 ) ;
#22849 = CARTESIAN_POINT ( 'NONE',  ( -0.3613381517857143232, 0.4044642856167432465, -4.425116109941954795E-17 ) ) ;
#22850 = LINE ( 'NONE', #17133, #20884 ) ;
#22851 = DIMENSIONAL_EXPONENTS ( 1.000000000000000000, 0.000000000000000000, 0.000000000000000000, 0.000000000000000000, 0.000000000000000000, 0.000000000000000000, 0.000000000000000000 ) ;
#22852 = DIRECTION ( 'NONE',  ( -0.000000000000000000, -0.000000000000000000, -1.000000000000000000 ) ) ;
#22853 = CARTESIAN_POINT ( 'NONE',  ( 0.1167790944451424368, 3.925777777853643347, 0.2819296736111110424 ) ) ;
#22854 = CARTESIAN_POINT ( 'NONE',  ( -0.3100543665040827457, -0.3622559054007235546, 0.4143868288130764799 ) ) ;
#22855 = CARTESIAN_POINT ( 'NONE',  ( -0.2389227046462522874, 5.186592499910797294, 0.1656744875650611459 ) ) ;
#22856 = CARTESIAN_POINT ( 'NONE',  ( 0.1292346314604056190, 4.540361111262843252, -0.3119999999999999996 ) ) ;
#22857 = CARTESIAN_POINT ( 'NONE',  ( 0.1167790944451424506, 4.884111111186975940, 0.2819296736111110424 ) ) ;
#22858 = ORIENTED_EDGE ( 'NONE', *, *, #22032, .F. ) ;
#22859 = CARTESIAN_POINT ( 'NONE',  ( 0.1993543840281267465, 4.318138888964754507, 0.1993543840281266633 ) ) ;
#22860 = ORIENTED_EDGE ( 'NONE', *, *, #7333, .F. ) ;
#22861 = CARTESIAN_POINT ( 'NONE',  ( 2.326421213736078119E-17, 0.2973214284738861513, -0.3799334167787516980 ) ) ;
#22862 = EDGE_CURVE ( 'NONE', #8952, #6354, #800, .T. ) ;
#22863 = ORIENTED_EDGE ( 'NONE', *, *, #20735, .F. ) ;
#22864 = ORIENTED_EDGE ( 'NONE', *, *, #9482, .F. ) ;
#22865 = DATE_AND_TIME ( #8101, #978 ) ;
#22866 =( BOUNDED_CURVE ( )  B_SPLINE_CURVE ( 2, ( #22122, #9079, #13007, #5421, #12522, #3715, #16410, #3351, #23818 ),
 .UNSPECIFIED., .F., .F. ) 
 B_SPLINE_CURVE_WITH_KNOTS ( ( 3, 2, 2, 2, 3 ),
 ( 0.4375000000000000000, 0.4479166666666666852, 0.4583333333333333148, 0.4687500000000000000, 0.4791666666666666852 ),
 .UNSPECIFIED. ) 
 CURVE ( )  GEOMETRIC_REPRESENTATION_ITEM ( )  RATIONAL_B_SPLINE_CURVE ( ( 1.000000000000000000, 0.9238795325112867385, 1.000000000000000000, 0.9238795325112867385, 1.000000000000000000, 0.9238795325112867385, 1.000000000000000000, 0.9238795325112867385, 1.000000000000000000 ) ) 
 REPRESENTATION_ITEM ( '' )  );
#22867 = CARTESIAN_POINT ( 'NONE',  ( 0.3394572874457115752, 3.700000000000000622, -0.09499999999999993172 ) ) ;
#22868 = CARTESIAN_POINT ( 'NONE',  ( 0.000000000000000000, 0.3125000000000000000, 0.2688888888888920636 ) ) ;
#22869 = CARTESIAN_POINT ( 'NONE',  ( -0.2206173157302028787, 0.04583333318160039832, 0.2206173157302027954 ) ) ;
#22870 = CARTESIAN_POINT ( 'NONE',  ( 0.2736220506547213938, 4.414403590476274175, 0.1516610675028668143 ) ) ;
#22871 = CARTESIAN_POINT ( 'NONE',  ( 0.1954553509668047195, 0.1954553509668046085, 0.1786111111111137462 ) ) ;
#22872 = CARTESIAN_POINT ( 'NONE',  ( -0.2819296736111110979, 0.4104166665908000056, -3.452642723725051716E-17 ) ) ;
#22873 = CARTESIAN_POINT ( 'NONE',  ( -0.1144950937579609918, -0.2764156081756484196, -0.1234722222222220528 ) ) ;
#22874 = ORIENTED_EDGE ( 'NONE', *, *, #1536, .T. ) ;
#22875 = CARTESIAN_POINT ( 'NONE',  ( -0.2819296736111110979, 4.811194444520309865, 0.000000000000000000 ) ) ;
#22876 = CARTESIAN_POINT ( 'NONE',  ( 0.006494592121999842073, -0.5491884613158954931, 0.04193801346286461784 ) ) ;
#22877 = CARTESIAN_POINT ( 'NONE',  ( 5.178964085587577574E-17, 4.700083333409199149, 0.2819296736111110979 ) ) ;
#22878 = ADVANCED_FACE ( 'NONE', ( #19817 ), #15798, .T. ) ;
#22879 = CARTESIAN_POINT ( 'NONE',  ( 0.2779722363314617861, 4.867466925649863718, -0.1418491738069263541 ) ) ;
#22880 = DIRECTION ( 'NONE',  ( 0.8660254037844360431, 0.000000000000000000, 0.5000000000000043299 ) ) ;
#22881 = FACE_OUTER_BOUND ( 'NONE', #21394, .T. ) ;
#22882 = CARTESIAN_POINT ( 'NONE',  ( -0.3119999999999999996, 4.384111111111110404, 0.000000000000000000 ) ) ;
#22883 = EDGE_CURVE ( 'NONE', #17619, #5247, #11918, .T. ) ;
#22884 = AXIS2_PLACEMENT_3D ( 'NONE', #19704, #12410, #695 ) ;
#22885 = CARTESIAN_POINT ( 'NONE',  ( 0.1167790944451422702, 3.891055555631421470, -0.2819296736111110979 ) ) ;
#22886 = CARTESIAN_POINT ( 'NONE',  ( -1.910449006669871087E-17, 4.703555555555555046, -0.3119999999999999996 ) ) ;
#22887 = ORIENTED_EDGE ( 'NONE', *, *, #23237, .T. ) ;
#22888 = CARTESIAN_POINT ( 'NONE',  ( 2.802071455580988509E-07, 4.599388881221821990, -0.3119999999998741003 ) ) ;
#22889 = EDGE_LOOP ( 'NONE', ( #12153, #8039, #17121, #306 ) ) ;
#22890 = EDGE_CURVE ( 'NONE', #5468, #14944, #16037, .T. ) ;
#22891 = CARTESIAN_POINT ( 'NONE',  ( 0.2666049204415198437, 4.701487312746555958, -0.1626043098652351082 ) ) ;
#22892 = UNCERTAINTY_MEASURE_WITH_UNIT (LENGTH_MEASURE( 1.000000000000000082E-05 ), #6246, 'distance_accuracy_value', 'NONE');
#22893 = LINE ( 'NONE', #8366, #14269 ) ;
#22894 = CARTESIAN_POINT ( 'NONE',  ( -0.2230971623002953874, 0.2230971623002954152, -0.1078472222222217058 ) ) ;
#22895 = AXIS2_PLACEMENT_3D ( 'NONE', #9956, #19091, #13622 ) ;
#22896 = CARTESIAN_POINT ( 'NONE',  ( 0.3125000000000000000, -5.740531871003217465E-17, 0.1438888888888910089 ) ) ;
#22897 = ORIENTED_EDGE ( 'NONE', *, *, #8017, .T. ) ;
#22898 = CARTESIAN_POINT ( 'NONE',  ( 0.3613381517857143232, 0.4366071427596004417, 0.1174058825155742114 ) ) ;
#22899 = CARTESIAN_POINT ( 'NONE',  ( -0.2819296736111110979, 0.5076388888130222155, -3.452642723725051716E-17 ) ) ;
#22900 = DIRECTION ( 'NONE',  ( 1.000000000000000000, 0.000000000000000000, -1.224646799147353207E-16 ) ) ;
#22901 = LINE ( 'NONE', #13414, #14690 ) ;
#22902 = CARTESIAN_POINT ( 'NONE',  ( -0.3065849364905382513, 4.708020935245015622E-15, -0.09575160315720471216 ) ) ;
#22903 = CARTESIAN_POINT ( 'NONE',  ( -0.1954553509668046918, -0.1954553509668046640, 0.1022222222222241989 ) ) ;
#22904 = ORIENTED_EDGE ( 'NONE', *, *, #1590, .F. ) ;
#22905 = CARTESIAN_POINT ( 'NONE',  ( -0.1497743226700191388, 4.622716354764487612, 0.2736999939638214974 ) ) ;
#22906 = PLANE ( 'NONE',  #23362 ) ;
#22907 = CYLINDRICAL_SURFACE ( 'NONE', #6333, 0.3119999999999999996 ) ;
#22908 = CARTESIAN_POINT ( 'NONE',  ( 0.3119999999999999996, 0.2993055555555552139, -0.1292346314604056468 ) ) ;
#22909 = CARTESIAN_POINT ( 'NONE',  ( 0.3119999999999999996, 4.856333333333332725, -3.820898013339742174E-17 ) ) ;
#22910 = CARTESIAN_POINT ( 'NONE',  ( -0.2819296736111110424, 4.314666666742533074, 0.1167790944451424923 ) ) ;
#22911 = CARTESIAN_POINT ( 'NONE',  ( -0.3038293207672896901, 4.337833751873854560, 0.08185879226206393966 ) ) ;
#22912 = CARTESIAN_POINT ( 'NONE',  ( -0.02441201398332129568, 4.111524471938507119, -3.542879552481994043 ) ) ;
#22913 = B_SPLINE_CURVE_WITH_KNOTS ( 'NONE', 3,
 ( #5283, #18575, #1866, #7245, #5527, #18692, #9428, #7596, #8946, #5768, #20405, #3698, #22109, #14811, #5404, #13228, #7360, #18452, #15048, #18335 ),
 .UNSPECIFIED., .F., .F.,
 ( 4, 2, 2, 2, 2, 2, 2, 2, 2, 4 ),
 ( 0.8497888536353912503, 0.8505139355485479280, 0.8512390174617047167, 0.8526891812880181831, 0.8541393451143315385, 0.8555895089406450049, 0.8570396727669584713, 0.8584898365932718267, 0.8599400004195852931, 0.8613901642458987595 ),
 .UNSPECIFIED. ) ;
#22914 = CARTESIAN_POINT ( 'NONE',  ( 0.2786222087057687591, 1.697684548454547126E-17, 0.2312824624941703378 ) ) ;
#22915 = EDGE_LOOP ( 'NONE', ( #5584, #17113 ) ) ;
#22916 = AXIS2_PLACEMENT_3D ( 'NONE', #23634, #21816, #5106 ) ;
#22917 = CARTESIAN_POINT ( 'NONE',  ( -0.4805456235326251990, -0.2624941757204518611, 0.04270874187135761946 ) ) ;
#22918 = EDGE_CURVE ( 'NONE', #2004, #19258, #20378, .T. ) ;
#22919 = CARTESIAN_POINT ( 'NONE',  ( -0.2819296736111110979, 4.741750000075865223, 0.000000000000000000 ) ) ;
#22920 = CARTESIAN_POINT ( 'NONE',  ( 0.1116596296178199027, 0.4080357141881718608, 0.3436530038418508792 ) ) ;
#22921 = LINE ( 'NONE', #20973, #16156 ) ;
#22922 = APPROVAL_ROLE ( '' ) ;
#22923 = CARTESIAN_POINT ( 'NONE',  ( -0.4687500000000003886, 0.2150880996501464693, 0.05816232583285784602 ) ) ;
#22924 = PLANE ( 'NONE',  #13055 ) ;
#22925 = CARTESIAN_POINT ( 'NONE',  ( -0.2819296736111110979, 4.366750000075866112, 0.000000000000000000 ) ) ;
#22926 = CARTESIAN_POINT ( 'NONE',  ( -0.0002931826408786237289, 4.043841211789635182, -0.3119998970421027362 ) ) ;
#22927 = CARTESIAN_POINT ( 'NONE',  ( -0.2764156081756484196, -0.1144950937579609362, -0.01236111111111004406 ) ) ;
#22928 = DIRECTION ( 'NONE',  ( 0.5000000000000007772, 0.000000000000000000, 0.8660254037844382635 ) ) ;
#22929 = CONICAL_SURFACE ( 'NONE', #17487, 0.7500000000000001110, 0.7853981633974482790 ) ;
#22930 = CARTESIAN_POINT ( 'NONE',  ( 0.1993543840281266355, 0.3756944443685777402, 0.1993543840281267465 ) ) ;
#22931 = FACE_OUTER_BOUND ( 'NONE', #10405, .T. ) ;
#22932 = CARTESIAN_POINT ( 'NONE',  ( 0.000000000000000000, 0.06249999999999967387, 0.000000000000000000 ) ) ;
#22933 = CARTESIAN_POINT ( 'NONE',  ( -0.3155070326520292845, 1.931923388228935888E-17, 0.06229166666666812596 ) ) ;
#22934 = CYLINDRICAL_SURFACE ( 'NONE', #15344, 0.2499999999999999722 ) ;
#22935 = CARTESIAN_POINT ( 'NONE',  ( -0.3119984077913639520, 3.778846792292107182, -0.04085387950071681790 ) ) ;
#22936 = CARTESIAN_POINT ( 'NONE',  ( -0.1167790944451422702, 0.4972222221463556413, -0.2819296736111110979 ) ) ;
#22937 = CARTESIAN_POINT ( 'NONE',  ( -0.1993543840281267465, 0.1256944443685777957, 0.1993543840281266633 ) ) ;
#22938 = CARTESIAN_POINT ( 'NONE',  ( 5.178964085587577574E-17, 4.325083333409199149, 0.2819296736111110979 ) ) ;
#22939 = CARTESIAN_POINT ( 'NONE',  ( -0.1236067977499789583, 0.2696428569477723469, -0.3804226065180614791 ) ) ;
#22940 = CARTESIAN_POINT ( 'NONE',  ( 0.1993543840281266633, 4.790361111186976828, -0.1993543840281266910 ) ) ;
#22941 = CARTESIAN_POINT ( 'NONE',  ( -0.3125000000000004996, -0.1294417382415916640, 0.2931944444444481435 ) ) ;
#22942 = ORIENTED_EDGE ( 'NONE', *, *, #15431, .T. ) ;
#22943 = CARTESIAN_POINT ( 'NONE',  ( -0.3119999999999999996, 3.832027777929509771, -0.1292346314604056468 ) ) ;
#22944 = CARTESIAN_POINT ( 'NONE',  ( -8.252060436089559755E-07, 4.682689096385127314, 0.3119999999976427185 ) ) ;
#22945 = TOROIDAL_SURFACE ( 'NONE', #21783, 0.2510000000000000009, 0.0009999999999999896125 ) ;
#22946 = ORIENTED_EDGE ( 'NONE', *, *, #8802, .T. ) ;
#22947 = DATE_AND_TIME ( #13593, #7243 ) ;
#22948 = CARTESIAN_POINT ( 'NONE',  ( 0.3236067977499789694, 0.3214285714285713413, 0.2351141009169893659 ) ) ;
#22949 = CARTESIAN_POINT ( 'NONE',  ( -0.5116234456863258950, 1.487605717019675700, -2.640781157734872320 ) ) ;
#22950 = ORIENTED_EDGE ( 'NONE', *, *, #935, .F. ) ;
#22951 = CARTESIAN_POINT ( 'NONE',  ( 0.1993543840281266355, 0.09791666659080004720, 0.1993543840281267465 ) ) ;
#22952 = ORIENTED_EDGE ( 'NONE', *, *, #21395, .T. ) ;
#22953 = CARTESIAN_POINT ( 'NONE',  ( 0.1569321314460191408, 4.242963909200604178, 0.2727264845398821858 ) ) ;
#22954 = ADVANCED_FACE ( 'NONE', ( #2861 ), #2011, .T. ) ;
#22955 = CARTESIAN_POINT ( 'NONE',  ( 0.2720287551442869267, 0.3842100023554017030, 0.4182004018663288414 ) ) ;
#22956 = CARTESIAN_POINT ( 'NONE',  ( 0.2754387896051087581, 4.081160839835338727, 0.1498674073576002908 ) ) ;
#22957 = CARTESIAN_POINT ( 'NONE',  ( 0.3613381517857143232, 0.2794642856167433020, 0.000000000000000000 ) ) ;
#22958 = CARTESIAN_POINT ( 'NONE',  ( 0.4450000000000002842, 0.000000000000000000, -2.540999999999999925 ) ) ;
#22959 = VECTOR ( 'NONE', #20895, 39.37007874015748143 ) ;
#22960 = ORIENTED_EDGE ( 'NONE', *, *, #9157, .T. ) ;
#22961 = CARTESIAN_POINT ( 'NONE',  ( -6.979263641208234666E-17, 0.3508928570453145879, 0.3799334167787516980 ) ) ;
#22962 = AXIS2_PLACEMENT_3D ( 'NONE', #11179, #13143, #14845 ) ;
#22963 = CARTESIAN_POINT ( 'NONE',  ( -0.2020650928029223692, -0.4371048157571741921, 0.07438423612653363715 ) ) ;
#22964 = CC_DESIGN_PERSON_AND_ORGANIZATION_ASSIGNMENT ( #4058, #17353, ( #3495 ) ) ;
#22965 = CARTESIAN_POINT ( 'NONE',  ( -0.2819296736111110424, 4.071611111186976828, -0.1167790944451423119 ) ) ;
#22966 = CARTESIAN_POINT ( 'NONE',  ( 0.06090617276557083043, 5.042162600288494723, -0.3064239527462913615 ) ) ;
#22967 = CARTESIAN_POINT ( 'NONE',  ( 0.000000000000000000, 0.4997679491924311157, 0.000000000000000000 ) ) ;
#22968 = CARTESIAN_POINT ( 'NONE',  ( 0.1292346314604058410, 4.463972222373954857, 0.3119999999999998885 ) ) ;
#22969 = CARTESIAN_POINT ( 'NONE',  ( 0.1993543840281267465, 4.943138888964754507, 0.1993543840281266633 ) ) ;
#22970 = ORIENTED_EDGE ( 'NONE', *, *, #23118, .F. ) ;
#22971 = CARTESIAN_POINT ( 'NONE',  ( 5.178964085587577574E-17, 4.144527777853642903, 0.2819296736111110979 ) ) ;
#22972 = CARTESIAN_POINT ( 'NONE',  ( -0.3613381517857143232, 0.2401785713310289616, -0.1174058825155741143 ) ) ;
#22973 = ORIENTED_EDGE ( 'NONE', *, *, #19752, .F. ) ;
#22974 = VECTOR ( 'NONE', #10120, 39.37007874015748143 ) ;
#22975 = VERTEX_POINT ( 'NONE', #10922 ) ;
#22976 = COORDINATED_UNIVERSAL_TIME_OFFSET ( 0, 0, .AHEAD. ) ;
#22977 = PLANE ( 'NONE',  #20054 ) ;
#22978 = FACE_OUTER_BOUND ( 'NONE', #21642, .T. ) ;
#22979 = CARTESIAN_POINT ( 'NONE',  ( 0.4587684526354154357, 0.1777979193111714762, 0.4165948764943589455 ) ) ;
#22980 = CARTESIAN_POINT ( 'NONE',  ( 0.03975918008867412173, 5.131473312690730815, 0.3040444178253544072 ) ) ;
#22981 = EDGE_CURVE ( 'NONE', #22355, #2961, #14581, .T. ) ;
#22982 = CARTESIAN_POINT ( 'NONE',  ( 0.06319114465426710348, 4.406713632401503489, 0.3055443619506773012 ) ) ;
#22983 = CARTESIAN_POINT ( 'NONE',  ( 1.910449006669871087E-17, 0.08055555540382261515, -0.3119999999999999996 ) ) ;
#22984 = CARTESIAN_POINT ( 'NONE',  ( 0.009375000000000025674, -0.5358532185916218271, 0.06112444011295370405 ) ) ;
#22985 = CARTESIAN_POINT ( 'NONE',  ( -3.385114897866767815E-17, -0.2764156081756484196, 0.2688888888888921747 ) ) ;
#22986 = CARTESIAN_POINT ( 'NONE',  ( 1.726321361862525858E-17, 0.1048611110352444808, -0.2819296736111110979 ) ) ;
#22987 = CARTESIAN_POINT ( 'NONE',  ( -0.1954553509668046640, 0.1954553509668046918, 0.4216666666666711305 ) ) ;
#22988 = VERTEX_POINT ( 'NONE', #11164 ) ;
#22989 = CARTESIAN_POINT ( 'NONE',  ( 0.2819296736111110979, 4.779944444520310753, 0.1167790944451422425 ) ) ;
#22990 = DIRECTION ( 'NONE',  ( 0.000000000000000000, 0.000000000000000000, -1.000000000000000000 ) ) ;
#22991 = ADVANCED_FACE ( 'NONE', ( #7376 ), #10805, .T. ) ;
#22992 = CARTESIAN_POINT ( 'NONE',  ( 0.1993543840281267465, 4.762583333409199149, 0.1993543840281266633 ) ) ;
#22993 = CARTESIAN_POINT ( 'NONE',  ( -0.002224882015017722817, 4.155008342873060201, -0.3119932009208763457 ) ) ;
#22994 = CARTESIAN_POINT ( 'NONE',  ( 0.2209708691207961095, -0.2209708691207961651, 0.3591666666666705199 ) ) ;
#22995 = DIRECTION ( 'NONE',  ( 0.000000000000000000, 0.000000000000000000, 1.000000000000000000 ) ) ;
#22996 = DIRECTION ( 'NONE',  ( -0.5000000000000007772, 1.043468761970410837E-18, -0.8660254037844380415 ) ) ;
#22997 = CARTESIAN_POINT ( 'NONE',  ( -0.1292346314604057023, 4.283416666666666650, 0.3119999999999998885 ) ) ;
#22998 = AXIS2_PLACEMENT_3D ( 'NONE', #13289, #16924, #5582 ) ;
#22999 = CARTESIAN_POINT ( 'NONE',  ( 0.3119999999999999996, 5.088972222373954857, -0.1292346314604056745 ) ) ;
#23000 = CARTESIAN_POINT ( 'NONE',  ( -0.3255746763033851021, 3.686631053841027850, 0.09499999999999995948 ) ) ;
#23001 = ORIENTED_EDGE ( 'NONE', *, *, #17834, .F. ) ;
#23002 = CARTESIAN_POINT ( 'NONE',  ( 0.000000000000000000, 0.3125000000000000000, 0.2133333333333360116 ) ) ;
#23003 = ORIENTED_EDGE ( 'NONE', *, *, #8703, .F. ) ;
#23004 =( BOUNDED_CURVE ( )  B_SPLINE_CURVE ( 2, ( #503, #22818, #21235, #11989, #21355, #10151, #8415, #4643, #14041 ),
 .UNSPECIFIED., .F., .T. ) 
 B_SPLINE_CURVE_WITH_KNOTS ( ( 3, 2, 2, 2, 3 ),
 ( 0.2291666666666667407, 0.2395833333333334259, 0.2500000000000001110, 0.2604166666666667962, 0.2708333333333334259 ),
 .UNSPECIFIED. ) 
 CURVE ( )  GEOMETRIC_REPRESENTATION_ITEM ( )  RATIONAL_B_SPLINE_CURVE ( ( 0.9999999999999994449, 0.9238795325112872936, 1.000000000000000000, 0.9238795325112867385, 1.000000000000000000, 0.9238795325112867385, 1.000000000000000000, 0.9238795325112859613, 1.000000000000000888 ) ) 
 REPRESENTATION_ITEM ( '' )  );
#23005 =( BOUNDED_SURFACE ( )  B_SPLINE_SURFACE ( 3, 2, ( 
 ( #15839, #3036, #17671 ),
 ( #12084, #8639, #19255 ),
 ( #19735, #16084, #12321 ),
 ( #23497, #15606, #19494 ),
 ( #23379, #724, #6567 ),
 ( #2676, #2789, #14017 ),
 ( #956, #1083, #21448 ),
 ( #6688, #2560, #14133 ),
 ( #21563, #4377, #10008 ),
 ( #17431, #17551, #23027 ),
 ( #6328, #21208, #4500 ),
 ( #845, #1569, #20103 ) ),
 .UNSPECIFIED., .F., .F., .F. ) 
 B_SPLINE_SURFACE_WITH_KNOTS ( ( 4, 2, 2, 2, 2, 4 ),
 ( 3, 3 ),
 ( 0.001926919177646338422, 0.005264799389783186324, 0.006933739495851611034, 0.008602679601920034877, 0.01194055981405688430, 0.01527844002619373198 ),
 ( 0.000000000000000000, 1.000000000000000000 ),
 .UNSPECIFIED. ) 
 GEOMETRIC_REPRESENTATION_ITEM ( )  RATIONAL_B_SPLINE_SURFACE ( (
 ( 1.000000000000000000, 0.8464669816041905381, 1.000000000000000000),
 ( 1.000000000000000000, 0.8516517675253432174, 1.000000000000000000),
 ( 1.000000000000000000, 0.8565844288627803005, 1.000000000000000000),
 ( 1.000000000000000000, 0.8620057511681040729, 1.000000000000000000),
 ( 1.000000000000000000, 0.8634777350187821110, 1.000000000000000000),
 ( 1.000000000000000000, 0.8654907715252899703, 1.000000000000000000),
 ( 1.000000000000000000, 0.8660271740515483874, 1.000000000000000000),
 ( 1.000000000000000000, 0.8660218497380072211, 1.000000000000000000),
 ( 1.000000000000000000, 0.8638283365559921156, 1.000000000000000000),
 ( 1.000000000000000000, 0.8566178551150570586, 1.000000000000000000),
 ( 1.000000000000000000, 0.8516788886409425441, 1.000000000000000000),
 ( 1.000000000000000000, 0.8464669816041904271, 1.000000000000000000) ) ) 
 REPRESENTATION_ITEM ( '' )  SURFACE ( )  );
#23006 = CARTESIAN_POINT ( 'NONE',  ( 0.001521130329658632301, 4.710459113145087251, -0.3119968249152551554 ) ) ;
#23007 = CARTESIAN_POINT ( 'NONE',  ( -2.918002456435568987E-09, 4.127166543308980806, 0.3119999999999999996 ) ) ;
#23008 = EDGE_CURVE ( 'NONE', #314, #8442, #149, .T. ) ;
#23009 = CARTESIAN_POINT ( 'NONE',  ( 0.1306872919485616846, 0.3155070326520292290, 0.1039583333333355397 ) ) ;
#23010 = ADVANCED_FACE ( 'NONE', ( #5303 ), #23696, .T. ) ;
#23011 = CARTESIAN_POINT ( 'NONE',  ( -0.1060554323913586589, 3.514980167629567998, 2.783525011231007706 ) ) ;
#23012 = CARTESIAN_POINT ( 'NONE',  ( -0.2923287055106771337, 0.02232142847388617762, -0.2123892367102620804 ) ) ;
#23013 = CARTESIAN_POINT ( 'NONE',  ( -0.2819296736111110424, 0.4486111110352445364, -0.1167790944451423396 ) ) ;
#23014 = CARTESIAN_POINT ( 'NONE',  ( -0.03651601414465285855, -0.2739930093161157543, -0.06558227484231510251 ) ) ;
#23015 = CARTESIAN_POINT ( 'NONE',  ( 0.2502152602304669737, 0.002284799041592490421, 0.2703534214026953597 ) ) ;
#23016 = CARTESIAN_POINT ( 'NONE',  ( -0.03651601414465285855, -0.2739930093161157543, -0.06558227484231510251 ) ) ;
#23017 = CARTESIAN_POINT ( 'NONE',  ( -0.1144950937579609918, -0.2764156081756484196, 0.2723611111111143845 ) ) ;
#23018 = EDGE_CURVE ( 'NONE', #10793, #14891, #22866, .T. ) ;
#23019 = VERTEX_POINT ( 'NONE', #19941 ) ;
#23020 = CARTESIAN_POINT ( 'NONE',  ( -0.1808653720604334325, 5.113170069492856129, 0.2512378506988575122 ) ) ;
#23021 = CARTESIAN_POINT ( 'NONE',  ( 1.750236327630675537E-16, 0.08749999980491518503, 0.3999999999999999667 ) ) ;
#23022 = CARTESIAN_POINT ( 'NONE',  ( 0.000000000000000000, 0.9300000000000000488, 0.000000000000000000 ) ) ;
#23023 = CARTESIAN_POINT ( 'NONE',  ( -0.2206173157302028787, 0.5527777777777773682, 0.2206173157302027954 ) ) ;
#23024 = CARTESIAN_POINT ( 'NONE',  ( 0.1292346314604058410, 5.012583333333332725, 0.3119999999999998885 ) ) ;
#23025 = CARTESIAN_POINT ( 'NONE',  ( -0.1167790944451423257, 4.023000000075866112, -0.2819296736111110424 ) ) ;
#23026 = DIRECTION ( 'NONE',  ( 1.000000000000000000, 0.000000000000000000, -0.000000000000000000 ) ) ;
#23027 = CARTESIAN_POINT ( 'NONE',  ( -0.08316635082768847331, 0.4932497623273897069, 0.4003041662012485902 ) ) ;
#23028 = CARTESIAN_POINT ( 'NONE',  ( 0.4500000000000003442, -0.2598076211353317344, 0.4425000000000000044 ) ) ;
#23029 = EDGE_LOOP ( 'NONE', ( #20374, #24070, #23085, #3230 ) ) ;
#23030 = LINE ( 'NONE', #8391, #21003 ) ;
#23031 = CARTESIAN_POINT ( 'NONE',  ( -0.1167790944451423535, 4.696611111186976828, 0.2819296736111110424 ) ) ;
#23032 = CARTESIAN_POINT ( 'NONE',  ( -0.1116596296178200276, 0.3294642856167432354, 0.3436530038418508792 ) ) ;
#23033 = CARTESIAN_POINT ( 'NONE',  ( -0.2614063550833075067, 5.159425771521426896, 0.1481041763251536303 ) ) ;
#23034 = DATE_AND_TIME ( #6216, #13444 ) ;
#23035 = CARTESIAN_POINT ( 'NONE',  ( 0.1527521626045861280, 0.4420638983541222977, 0.4298724737630856829 ) ) ;
#23036 = DIRECTION ( 'NONE',  ( -0.8635502596144278842, -0.07555085810113110201, -0.4985709748471494618 ) ) ;
#23037 = CARTESIAN_POINT ( 'NONE',  ( 0.1167790944451422702, 4.293833333409199149, -0.2819296736111110979 ) ) ;
#23038 = APPROVAL_STATUS ( 'not_yet_approved' ) ;
#23039 = CARTESIAN_POINT ( 'NONE',  ( -0.08351110729652544418, 4.046178605385413185, -0.3012663639467730858 ) ) ;
#23040 = CARTESIAN_POINT ( 'NONE',  ( 0.1954553509668047195, 0.1954553509668046085, 0.2966666666666701313 ) ) ;
#23041 = CARTESIAN_POINT ( 'NONE',  ( 0.2209708691207961095, -0.2209708691207961651, 0.3661111111111154393 ) ) ;
#23042 = APPLICATION_CONTEXT ( 'configuration controlled 3d designs of mechanical parts and assemblies' ) ;
#23043 = CARTESIAN_POINT ( 'NONE',  ( 1.726321361862525858E-17, 0.5076388888130222155, -0.2819296736111110979 ) ) ;
#23044 = DIRECTION ( 'NONE',  ( 0.000000000000000000, 0.000000000000000000, -1.000000000000000000 ) ) ;
#23045 = CARTESIAN_POINT ( 'NONE',  ( 0.3124999999999996669, 0.1294417382415925521, -0.01930555555555471536 ) ) ;
#23046 = CARTESIAN_POINT ( 'NONE',  ( -0.3155070326520293400, 0.1306872919485614903, 0.05881944444444586056 ) ) ;
#23047 = CARTESIAN_POINT ( 'NONE',  ( 0.000000000000000000, 0.01999999999999951469, -1.243000000000000105 ) ) ;
#23048 = CARTESIAN_POINT ( 'NONE',  ( -0.2495005081859424656, 3.785671182798638235, 0.1917329975044681778 ) ) ;
#23049 = CARTESIAN_POINT ( 'NONE',  ( 0.2819296736111110979, 0.5388888888130223265, -0.1167790944451422980 ) ) ;
#23050 = CARTESIAN_POINT ( 'NONE',  ( -5.178964085587577574E-17, 0.2993055554796889561, 0.2819296736111110979 ) ) ;
#23051 = CARTESIAN_POINT ( 'NONE',  ( -0.1167790944451423257, 4.078555555631421470, -0.2819296736111110424 ) ) ;
#23052 = CARTESIAN_POINT ( 'NONE',  ( -0.4000000000000000222, 0.3553571426620580342, -4.898587196589413075E-17 ) ) ;
#23053 = AXIS2_PLACEMENT_3D ( 'NONE', #3692, #18445, #19921 ) ;
#23054 = CARTESIAN_POINT ( 'NONE',  ( 0.2819296736111110979, 4.724388888964754507, 0.1167790944451422425 ) ) ;
#23055 = CARTESIAN_POINT ( 'NONE',  ( -0.1292346314604056190, 0.1395833331816004053, -0.3119999999999999996 ) ) ;
#23056 = ORIENTED_EDGE ( 'NONE', *, *, #6029, .T. ) ;
#23057 = VERTEX_POINT ( 'NONE', #3471 ) ;
#23058 = CARTESIAN_POINT ( 'NONE',  ( 1.573500000000000343, 0.02500000000000021302, -0.5399999999999998135 ) ) ;
#23059 = CARTESIAN_POINT ( 'NONE',  ( -0.3119999999999999996, 3.779944444596176734, 0.000000000000000000 ) ) ;
#23060 = DIRECTION ( 'NONE',  ( 0.8660254037844523634, -0.000000000000000000, -0.4999999999999761857 ) ) ;
#23061 = SHAPE_REPRESENTATION_RELATIONSHIP ( 'NONE' , 'NONE' ,  #16955, #8245 ) ;
#23062 = VERTEX_POINT ( 'NONE', #23945 ) ;
#23063 = PERSON_AND_ORGANIZATION ( #15518, #2538 ) ;
#23064 = ORIENTED_EDGE ( 'NONE', *, *, #19301, .F. ) ;
#23065 = AXIS2_PLACEMENT_3D ( 'NONE', #17106, #11748, #4291 ) ;
#23066 = DIRECTION ( 'NONE',  ( -0.8660254037844434816, -0.000000000000000000, 0.4999999999999915068 ) ) ;
#23067 = CARTESIAN_POINT ( 'NONE',  ( -0.2983450752461472288, 4.999556594882858640, -0.09148912044693334467 ) ) ;
#23068 = CARTESIAN_POINT ( 'NONE',  ( 0.2206173157302028232, 0.6291666665149338034, -0.2206173157302028232 ) ) ;
#23069 = EDGE_LOOP ( 'NONE', ( #19738, #17261, #21593, #20767, #8340, #23761, #20252, #18531, #12323, #19588, #2984, #7168 ) ) ;
#23070 = CARTESIAN_POINT ( 'NONE',  ( 0.1127385644800980580, 4.262880112112297226, -0.2914991025335854635 ) ) ;
#23071 = CARTESIAN_POINT ( 'NONE',  ( 0.1568404389086313078, 0.4507140077415570656, 0.4133480672483983431 ) ) ;
#23072 = CARTESIAN_POINT ( 'NONE',  ( 0.2058003546260330774, 4.078051603074912101, 0.2353791526578999371 ) ) ;
#23073 = CARTESIAN_POINT ( 'NONE',  ( 0.1116596296178199027, 0.3366071427596004084, 0.3436530038418508792 ) ) ;
#23074 = PLANE ( 'NONE',  #9286 ) ;
#23075 = ADVANCED_FACE ( 'NONE', ( #1762 ), #7140, .T. ) ;
#23076 = CARTESIAN_POINT ( 'NONE',  ( -6.979263641208234666E-17, 0.2794642856167432465, 0.3799334167787516980 ) ) ;
#23077 = CARTESIAN_POINT ( 'NONE',  ( 1.652571746775178596, 2.291712385858714285, -2.061529041877832480 ) ) ;
#23078 = CARTESIAN_POINT ( 'NONE',  ( 0.1993543840281267465, 3.762583333409198705, 0.1993543840281266633 ) ) ;
#23079 = DIRECTION ( 'NONE',  ( 0.000000000000000000, 0.000000000000000000, 1.000000000000000000 ) ) ;
#23080 = CARTESIAN_POINT ( 'NONE',  ( -0.2932553954330455737, 5.179855157894580842, 0.004433361297087813797 ) ) ;
#23081 = CARTESIAN_POINT ( 'NONE',  ( 0.000000000000000000, 2.690000000000002167, -2.986000000000000210 ) ) ;
#23082 = CARTESIAN_POINT ( 'NONE',  ( 5.731347020009612645E-17, 4.627166666818398610, 0.3119999999999999996 ) ) ;
#23083 = VECTOR ( 'NONE', #7975, 39.37007874015748143 ) ;
#23084 = CARTESIAN_POINT ( 'NONE',  ( 5.178964085587577574E-17, 5.047305555631421470, 0.2819296736111110979 ) ) ;
#23085 = ORIENTED_EDGE ( 'NONE', *, *, #6620, .T. ) ;
#23086 = CARTESIAN_POINT ( 'NONE',  ( -0.2819296736111110424, 4.127166666742532186, -0.1167790944451423119 ) ) ;
#23087 = ORIENTED_EDGE ( 'NONE', *, *, #6038, .T. ) ;
#23088 = CARTESIAN_POINT ( 'NONE',  ( 0.2233192592356399164, 0.2687499999024575703, 0.3073725909049500604 ) ) ;
#23089 = ORIENTED_EDGE ( 'NONE', *, *, #16032, .T. ) ;
#23090 = APPROVAL_ROLE ( '' ) ;
#23091 = CC_DESIGN_PERSON_AND_ORGANIZATION_ASSIGNMENT ( #11847, #19264, ( #1355 ) ) ;
#23092 = CARTESIAN_POINT ( 'NONE',  ( 0.2209708691207961651, 0.2209708691207959985, 0.04666666666666840352 ) ) ;
#23093 = FACE_OUTER_BOUND ( 'NONE', #13546, .T. ) ;
#23094 = CARTESIAN_POINT ( 'NONE',  ( 0.3119999999999998885, 0.06319444429271152408, 0.1292346314604058410 ) ) ;
#23095 = CYLINDRICAL_SURFACE ( 'NONE', #394, 0.2109499999999996656 ) ;
#23096 = AXIS2_PLACEMENT_3D ( 'NONE', #14893, #4264, #19137 ) ;
#23097 = CARTESIAN_POINT ( 'NONE',  ( -0.4587622378227205200, -0.1787210847074471587, 0.4163997147010622402 ) ) ;
#23098 = DIRECTION ( 'NONE',  ( -0.000000000000000000, -1.000000000000000000, -0.000000000000000000 ) ) ;
#23099 = DIRECTION ( 'NONE',  ( 9.614813431917706176E-16, 0.7071067811865439090, -0.7071067811865511255 ) ) ;
#23100 = CARTESIAN_POINT ( 'NONE',  ( -0.2764156081756484196, -0.1144950937579609362, 0.3695833333333374826 ) ) ;
#23101 = CARTESIAN_POINT ( 'NONE',  ( -0.1993543840281267465, 0.07013888881302225708, 0.1993543840281266633 ) ) ;
#23102 = CARTESIAN_POINT ( 'NONE',  ( -3.385114897866767815E-17, -0.2764156081756484196, -0.008888888888887782128 ) ) ;
#23103 = FACE_OUTER_BOUND ( 'NONE', #22091, .T. ) ;
#23104 = CARTESIAN_POINT ( 'NONE',  ( -0.2819296736111110424, 4.689666666742532186, 0.1167790944451424923 ) ) ;
#23105 = CARTESIAN_POINT ( 'NONE',  ( 0.4593750000000000888, -0.04461821091738114864, 0.4343810118395100006 ) ) ;
#23106 = CARTESIAN_POINT ( 'NONE',  ( 3.857637417314162073E-17, 0.06786299768266475241, 0.3150000000000000022 ) ) ;
#23107 = LINE ( 'NONE', #13281, #11389 ) ;
#23108 = CARTESIAN_POINT ( 'NONE',  ( 8.904784892192170075E-17, -0.5196152422706635798, 0.3779506566538943235 ) ) ;
#23109 = CARTESIAN_POINT ( 'NONE',  ( 5.731347020009612645E-17, 4.286888888888888083, 0.3119999999999999996 ) ) ;
#23110 = CARTESIAN_POINT ( 'NONE',  ( 0.3125000000000000000, -5.740531871003217465E-17, 0.1438888888888910089 ) ) ;
#23111 = CARTESIAN_POINT ( 'NONE',  ( 0.3105037589794399921, 4.973547786746206789, 0.03065709337648704624 ) ) ;
#23112 = ADVANCED_FACE ( 'NONE', ( #20303 ), #8836, .T. ) ;
#23113 = CARTESIAN_POINT ( 'NONE',  ( 9.184850993605150903E-17, 0.9099999999999988098, -0.7500000000000001110 ) ) ;
#23114 = ORIENTED_EDGE ( 'NONE', *, *, #11008, .T. ) ;
#23115 = CARTESIAN_POINT ( 'NONE',  ( 0.000000000000000000, 3.669999999999999929, 0.000000000000000000 ) ) ;
#23116 = VERTEX_POINT ( 'NONE', #7261 ) ;
#23117 = CARTESIAN_POINT ( 'NONE',  ( 0.2485617479699924470, 4.690811910894372438, 0.1929793757338557625 ) ) ;
#23118 = EDGE_CURVE ( 'NONE', #12482, #795, #21255, .T. ) ;
#23119 = CARTESIAN_POINT ( 'NONE',  ( -9.626299801968715084E-16, 0.3464285714285713635, -0.4000000000000000222 ) ) ;
#23120 = CARTESIAN_POINT ( 'NONE',  ( 0.2230971623002953874, -0.2230971623002954429, 0.1421527777777802648 ) ) ;
#23121 = CARTESIAN_POINT ( 'NONE',  ( -0.04643773642726176792, -0.5144550377384379258, 0.07051021533369886130 ) ) ;
#23122 = CARTESIAN_POINT ( 'NONE',  ( -0.1116596296178200276, 0.04374999990245760639, 0.3436530038418508792 ) ) ;
#23123 = CARTESIAN_POINT ( 'NONE',  ( -0.1993543840281267465, 0.1395833332574666907, 0.1993543840281266633 ) ) ;
#23124 = CARTESIAN_POINT ( 'NONE',  ( -0.1954553509668046918, -0.1954553509668046640, -0.06444444444444380471 ) ) ;
#23125 = CARTESIAN_POINT ( 'NONE',  ( 9.184120737366631376E-17, 0.1556215347031258134, -0.7500000000000001110 ) ) ;
#23126 = CARTESIAN_POINT ( 'NONE',  ( 0.000000000000000000, 0.000000000000000000, 0.000000000000000000 ) ) ;
#23127 = AXIS2_PLACEMENT_3D ( 'NONE', #1918, #18747, #16804 ) ;
#23128 = ORIENTED_EDGE ( 'NONE', *, *, #18843, .T. ) ;
#23129 = CARTESIAN_POINT ( 'NONE',  ( -0.2975325615348068942, 4.615999354583628644, 0.09627391117643818719 ) ) ;
#23130 = CARTESIAN_POINT ( 'NONE',  ( -0.02459558260538192292, 4.293134600018148284, 0.3110673077616819548 ) ) ;
#23131 = CARTESIAN_POINT ( 'NONE',  ( 0.3125000000000000000, -5.740531871003217465E-17, 0.3175000000000038347 ) ) ;
#23132 = CARTESIAN_POINT ( 'NONE',  ( 0.2206173157302027676, 0.4555555555555552139, 0.2206173157302028787 ) ) ;
#23133 = CARTESIAN_POINT ( 'NONE',  ( -0.3119999999999999996, 4.939666666666665762, 0.000000000000000000 ) ) ;
#23134 = CARTESIAN_POINT ( 'NONE',  ( -0.1993543840281266355, 4.040361111186976828, 0.1993543840281267465 ) ) ;
#23135 =( BOUNDED_SURFACE ( )  B_SPLINE_SURFACE ( 3, 2, ( 
 ( #14036, #3166, #16225 ),
 ( #14395, #8899, #7077 ),
 ( #21819, #5109, #12575 ),
 ( #21466, #19996, #1101 ),
 ( #3284, #10738, #12221 ),
 ( #12104, #2807, #10262 ),
 ( #10388, #19631, #17810 ),
 ( #8534, #14765, #24120 ),
 ( #16582, #9137, #108 ),
 ( #9021, #3530, #7671 ) ),
 .UNSPECIFIED., .F., .F., .T. ) 
 B_SPLINE_SURFACE_WITH_KNOTS ( ( 4, 2, 2, 2, 4 ),
 ( 3, 3 ),
 ( 0.04450355443756499191, 0.04782809616271448128, 0.05115263788786396371, 0.05447717961301344614, 0.05780172133816293550 ),
 ( 0.000000000000000000, 1.000000000000000000 ),
 .UNSPECIFIED. ) 
 GEOMETRIC_REPRESENTATION_ITEM ( )  RATIONAL_B_SPLINE_SURFACE ( (
 ( 1.000000000000000000, 0.8285407536241355952, 1.000000000000000000),
 ( 1.000000000000000000, 0.8326162293447895157, 1.000000000000000000),
 ( 1.000000000000000000, 0.8363774056812446345, 1.000000000000000000),
 ( 1.000000000000000000, 0.8417899530394342689, 1.000000000000000000),
 ( 1.000000000000000000, 0.8433914761756452494, 1.000000000000000000),
 ( 1.000000000000000000, 0.8433914154492313520, 1.000000000000000000),
 ( 1.000000000000000000, 0.8417897495747284076, 1.000000000000000000),
 ( 1.000000000000000000, 0.8363771423991239740, 1.000000000000000000),
 ( 1.000000000000000000, 0.8326160433687649354, 1.000000000000000000),
 ( 1.000000000000000000, 0.8285407536241354842, 1.000000000000000000) ) ) 
 REPRESENTATION_ITEM ( '' )  SURFACE ( )  );
#23136 = LINE ( 'NONE', #12438, #5372 ) ;
#23137 = CARTESIAN_POINT ( 'NONE',  ( 5.731347020009612645E-17, 3.897999999999999243, 0.3119999999999999996 ) ) ;
#23138 = DIRECTION ( 'NONE',  ( 0.000000000000000000, 1.000000000000000000, 0.000000000000000000 ) ) ;
#23139 =( BOUNDED_CURVE ( )  B_SPLINE_CURVE ( 2, ( #14883, #3777, #11220, #1941, #14004, #4722, #2894, #4252, #1070 ),
 .UNSPECIFIED., .F., .F. ) 
 B_SPLINE_CURVE_WITH_KNOTS ( ( 3, 2, 2, 2, 3 ),
 ( 0.2708333333333334259, 0.2812500000000001110, 0.2916666666666667407, 0.3020833333333333703, 0.3125000000000000555 ),
 .UNSPECIFIED. ) 
 CURVE ( )  GEOMETRIC_REPRESENTATION_ITEM ( )  RATIONAL_B_SPLINE_CURVE ( ( 0.9999999999999992228, 0.9238795325112875156, 1.000000000000000000, 0.9238795325112867385, 1.000000000000000000, 0.9238795325112867385, 1.000000000000000000, 0.9238795325112862944, 1.000000000000000444 ) ) 
 REPRESENTATION_ITEM ( '' )  );
#23140 = VERTEX_POINT ( 'NONE', #11040 ) ;
#23141 = ORIENTED_EDGE ( 'NONE', *, *, #6361, .F. ) ;
#23142 = CARTESIAN_POINT ( 'NONE',  ( -0.2494960473753227714, 3.996427622109653299, -0.1917385859694114847 ) ) ;
#23143 = CARTESIAN_POINT ( 'NONE',  ( -0.2819296736111110424, 4.634111111186976828, 0.1167790944451424923 ) ) ;
#23144 = CARTESIAN_POINT ( 'NONE',  ( 0.2233192592356399164, 0.3401785713310290227, 0.3073725909049500604 ) ) ;
#23145 = CARTESIAN_POINT ( 'NONE',  ( 0.4172595264191667486, 2.291712385858714285, -0.8269699969948853813 ) ) ;
#23146 = AXIS2_PLACEMENT_3D ( 'NONE', #17268, #19090, #72 ) ;
#23147 = EDGE_CURVE ( 'NONE', #14969, #11153, #18136, .T. ) ;
#23148 = CARTESIAN_POINT ( 'NONE',  ( 0.1334180974147631538, 0.4531173396632154349, 0.4271664148355319157 ) ) ;
#23149 = CARTESIAN_POINT ( 'NONE',  ( -0.1954553509668046640, 0.1954553509668046918, 0.08138888888889070361 ) ) ;
#23150 = CARTESIAN_POINT ( 'NONE',  ( -0.2819296736111110979, 4.363277777853643791, -0.1167790944451422980 ) ) ;
#23151 = CARTESIAN_POINT ( 'NONE',  ( -0.3104415801607898762, 4.834635239992220335, -0.03154143600449414719 ) ) ;
#23152 = CARTESIAN_POINT ( 'NONE',  ( 0.04820796449995154442, 5.072973651020436847, 0.3082531300064171864 ) ) ;
#23153 = CARTESIAN_POINT ( 'NONE',  ( -0.2764156081756484196, 0.1144950937579609918, 0.3140277777777814028 ) ) ;
#23154 = CC_DESIGN_APPROVAL ( #3590, ( #6872 ) ) ;
#23155 = CARTESIAN_POINT ( 'NONE',  ( 0.1294417382415921358, -0.3125000000000002220, 0.3626388888888931183 ) ) ;
#23156 = CARTESIAN_POINT ( 'NONE',  ( 0.2819296736111110424, 0.09444444436857780956, -0.1167790944451423119 ) ) ;
#23157 = CARTESIAN_POINT ( 'NONE',  ( -5.731347020009612645E-17, 0.1152777777777774515, 0.3119999999999999996 ) ) ;
#23158 = CARTESIAN_POINT ( 'NONE',  ( 0.2206173157302027954, 4.474388888888888083, -0.2206173157302028232 ) ) ;
#23159 = CARTESIAN_POINT ( 'NONE',  ( -0.3236067977499790249, 0.3714285714285713302, 0.2351141009169892271 ) ) ;
#23160 = CARTESIAN_POINT ( 'NONE',  ( 0.1306872919485614071, -0.3155070326520293955, 0.4685416666666713525 ) ) ;
#23161 = FACE_OUTER_BOUND ( 'NONE', #13665, .T. ) ;
#23162 = ADVANCED_FACE ( 'NONE', ( #9206 ), #11846, .T. ) ;
#23163 = CARTESIAN_POINT ( 'NONE',  ( -0.3125000000000000000, 0.1294417382415922468, 0.3904166666666707419 ) ) ;
#23164 = CARTESIAN_POINT ( 'NONE',  ( -0.2819296736111110979, 0.4520833332574666907, -3.452642723725051716E-17 ) ) ;
#23165 = CARTESIAN_POINT ( 'NONE',  ( -0.1167790944451422702, 0.4416666665908000611, -0.2819296736111110424 ) ) ;
#23166 = CARTESIAN_POINT ( 'NONE',  ( -0.1993543840281266910, 4.137583333409199149, -0.1993543840281266910 ) ) ;
#23167 = CARTESIAN_POINT ( 'NONE',  ( 0.2472135954999579166, 0.3089285712334866041, 0.3402603233408160732 ) ) ;
#23168 = B_SPLINE_CURVE_WITH_KNOTS ( 'NONE', 3,
 ( #16745, #7475, #8944, #7121, #24048, #14561, #16392, #10903, #22106, #1745, #5279, #3451, #12989, #7358, #6998, #23800, #3211, #12623, #27, #8818, #3696, #18333, #20041, #16267, #1628, #16509, #7242, #14688, #3571, #9185, #16629, #14808, #20403, #11142, #18572, #9304, #14924, #23678, #3329 ),
 .UNSPECIFIED., .F., .F.,
 ( 4, 2, 2, 2, 2, 2, 2, 2, 2, 2, 1, 2, 2, 2, 2, 2, 2, 2, 2, 4 ),
 ( 0.9594394450162125887, 0.9614297162944156483, 0.9624248519335172336, 0.9634199875726187079, 0.9644151232117202932, 0.9654102588508217675, 0.9664053944899233528, 0.9674005301290248271, 0.9683956657681264124, 0.9693908014072278867, 0.9695151933621155571, 0.9695773893395593923, 0.9696395853170033385, 0.9698883692267786794, 0.9703859370463294720, 0.9713810726854309463, 0.9723762083245325316, 0.9733713439636340059, 0.9743664796027355912, 0.9753616152418370655 ),
 .UNSPECIFIED. ) ;
#23169 = CIRCLE ( 'NONE', #3318, 0.2124999999999999944 ) ;
#23170 = CARTESIAN_POINT ( 'NONE',  ( -0.1993543840281266355, 4.707027777853643791, 0.1993543840281267465 ) ) ;
#23171 = CARTESIAN_POINT ( 'NONE',  ( -0.09145417301143905775, 0.5014751291207464323, 0.06110928887248364555 ) ) ;
#23172 = CARTESIAN_POINT ( 'NONE',  ( 0.3236067977499789694, 0.1696428569477723136, 0.2351141009169893659 ) ) ;
#23173 = EDGE_CURVE ( 'NONE', #23807, #19658, #6060, .T. ) ;
#23174 = EDGE_LOOP ( 'NONE', ( #14726, #23783, #8593, #13093 ) ) ;
#23175 = EDGE_CURVE ( 'NONE', #10339, #19216, #13801, .T. ) ;
#23176 = CARTESIAN_POINT ( 'NONE',  ( 0.1292346314604056190, 4.700083333333332725, -0.3119999999999999996 ) ) ;
#23177 = CARTESIAN_POINT ( 'NONE',  ( -0.2206173157302028232, 3.939666666818398610, -0.2206173157302028232 ) ) ;
#23178 = LOCAL_TIME ( 21, 9, 13.00000000000000000, #9316 ) ;
#23179 = CARTESIAN_POINT ( 'NONE',  ( 0.07226797383931020391, -0.2674160455369279932, 0.3880822748423151669 ) ) ;
#23180 = ADVANCED_FACE ( 'NONE', ( #4641 ), #17755, .T. ) ;
#23181 = DIRECTION ( 'NONE',  ( 0.000000000000000000, 0.000000000000000000, 1.000000000000000000 ) ) ;
#23182 = VERTEX_POINT ( 'NONE', #2810 ) ;
#23183 = SECURITY_CLASSIFICATION_LEVEL ( 'unclassified' ) ;
#23184 = VERTEX_POINT ( 'NONE', #10265 ) ;
#23185 = VECTOR ( 'NONE', #19822, 39.37007874015748143 ) ;
#23186 = CARTESIAN_POINT ( 'NONE',  ( 5.731347020009612645E-17, 4.786888888888888083, 0.3119999999999999996 ) ) ;
#23187 = CARTESIAN_POINT ( 'NONE',  ( -0.2683814352459896746, 4.552880090615864184, -0.1640201213671886316 ) ) ;
#23188 = ORIENTED_EDGE ( 'NONE', *, *, #21993, .T. ) ;
#23189 = CARTESIAN_POINT ( 'NONE',  ( -0.1167790944451422702, 0.06666666659080003332, -0.2819296736111110424 ) ) ;
#23190 = ORIENTED_EDGE ( 'NONE', *, *, #1615, .F. ) ;
#23191 = CARTESIAN_POINT ( 'NONE',  ( 6.089848770316828444E-07, 4.238302053322364316, 0.3119999999987258521 ) ) ;
#23192 = CARTESIAN_POINT ( 'NONE',  ( 0.000000000000000000, 0.000000000000000000, 1.326383476483184332 ) ) ;
#23193 = PLANE ( 'NONE',  #21434 ) ;
#23194 = CARTESIAN_POINT ( 'NONE',  ( -0.1116596296178199582, 0.3723214284738861068, -0.3436530038418508792 ) ) ;
#23195 = CARTESIAN_POINT ( 'NONE',  ( 0.000000000000000000, 2.735000000000000320, 0.7500000000000001110 ) ) ;
#23196 = APPROVAL_PERSON_ORGANIZATION ( #21607, #11811, #12244 ) ;
#23197 = DIRECTION ( 'NONE',  ( 0.4999999999999923395, -0.000000000000000000, 0.8660254037844431485 ) ) ;
#23198 = LINE ( 'NONE', #15894, #22216 ) ;
#23199 = CARTESIAN_POINT ( 'NONE',  ( 0.1993543840281266633, 3.776472222298087988, -0.1993543840281266910 ) ) ;
#23200 = CARTESIAN_POINT ( 'NONE',  ( 0.2761986883776191282, 5.034245972029707694, -0.1452648408779728950 ) ) ;
#23201 = CARTESIAN_POINT ( 'NONE',  ( -0.2835900173929711277, 5.176626687221649092, -0.08093004039994856902 ) ) ;
#23202 = AXIS2_PLACEMENT_3D ( 'NONE', #11803, #19225, #11933 ) ;
#23203 = CARTESIAN_POINT ( 'NONE',  ( 0.2206173157302027954, 4.536888889040620931, -0.2206173157302028232 ) ) ;
#23204 = CARTESIAN_POINT ( 'NONE',  ( 0.1993543840281266633, 4.623694444520309865, -0.1993543840281266910 ) ) ;
#23205 = CARTESIAN_POINT ( 'NONE',  ( 0.1167790944451422702, 4.002166666742532186, -0.2819296736111110424 ) ) ;
#23206 = VERTEX_POINT ( 'NONE', #17691 ) ;
#23207 = ADVANCED_FACE ( 'NONE', ( #17451 ), #8413, .T. ) ;
#23208 = EDGE_CURVE ( 'NONE', #14891, #12009, #14039, .T. ) ;
#23209 = VERTEX_POINT ( 'NONE', #4753 ) ;
#23210 = APPROVAL_PERSON_ORGANIZATION ( #7453, #619, #19149 ) ;
#23211 = DATE_AND_TIME ( #15792, #5280 ) ;
#23212 = ORIENTED_EDGE ( 'NONE', *, *, #18604, .T. ) ;
#23213 = CARTESIAN_POINT ( 'NONE',  ( -0.3125000000000000000, 1.913510623667739771E-17, 0.06750000000000189182 ) ) ;
#23214 = EDGE_CURVE ( 'NONE', #14906, #431, #610, .T. ) ;
#23215 = CARTESIAN_POINT ( 'NONE',  ( 0.3119999999999998885, 0.1187499998482670627, 0.1292346314604058410 ) ) ;
#23216 = VECTOR ( 'NONE', #4751, 39.37007874015748143 ) ;
#23217 = CARTESIAN_POINT ( 'NONE',  ( 1.145733547534701715E-12, 5.130222168000691418, 0.3067077167097377322 ) ) ;
#23218 = CARTESIAN_POINT ( 'NONE',  ( -0.4687500000000003886, 0.1747335358173341124, 0.4002814116603867212 ) ) ;
#23219 = CARTESIAN_POINT ( 'NONE',  ( -3.385114897866767815E-17, -0.2764156081756484196, 0.3800000000000042233 ) ) ;
#23220 = CARTESIAN_POINT ( 'NONE',  ( 0.2819296736111110979, 0.03398119426037962687, 0.04827834974809540325 ) ) ;
#23221 = CARTESIAN_POINT ( 'NONE',  ( 0.2764156081756483641, 0.1144950937579610056, -0.04708333333333254017 ) ) ;
#23222 = CARTESIAN_POINT ( 'NONE',  ( 0.000000000000000000, 0.9099999999999988098, 0.000000000000000000 ) ) ;
#23223 = CARTESIAN_POINT ( 'NONE',  ( -0.1993543840281266355, 4.526472222298087544, 0.1993543840281267465 ) ) ;
#23224 = CARTESIAN_POINT ( 'NONE',  ( 0.1900105704308386045, 5.206640035683666845, 0.2082794372640154323 ) ) ;
#23225 = CARTESIAN_POINT ( 'NONE',  ( -0.1399538861531764988, 0.7553620363409487837, -1.079965667524036776 ) ) ;
#23226 = CARTESIAN_POINT ( 'NONE',  ( 2.126433378146018960, 2.690142902515285428, -2.942657555934166780 ) ) ;
#23227 = FACE_OUTER_BOUND ( 'NONE', #16350, .T. ) ;
#23228 = CARTESIAN_POINT ( 'NONE',  ( 0.3119999999999999996, 4.193138888888888083, -0.1292346314604056745 ) ) ;
#23229 = CARTESIAN_POINT ( 'NONE',  ( 5.731347020009612645E-17, 4.564666666666665762, 0.3119999999999999996 ) ) ;
#23230 = CARTESIAN_POINT ( 'NONE',  ( 9.101228903679513089E-16, 0.3107142857142856096, 0.4000000000000000222 ) ) ;
#23231 = CARTESIAN_POINT ( 'NONE',  ( 0.1290452976441722188, 4.964245088727332167, 0.2846185331919179329 ) ) ;
#23232 = AXIS2_PLACEMENT_3D ( 'NONE', #11251, #14909, #7581 ) ;
#23233 = FACE_OUTER_BOUND ( 'NONE', #9412, .T. ) ;
#23234 = ORIENTED_EDGE ( 'NONE', *, *, #3105, .T. ) ;
#23235 = CARTESIAN_POINT ( 'NONE',  ( 0.0001071248759953418567, 4.710497121865020453, -0.3119999863294411480 ) ) ;
#23236 = CARTESIAN_POINT ( 'NONE',  ( 0.2557079804836105974, 4.135622660786435922, 0.1809013949627109874 ) ) ;
#23237 = EDGE_CURVE ( 'NONE', #789, #16124, #2463, .T. ) ;
#23238 = CARTESIAN_POINT ( 'NONE',  ( -0.3155070326520292845, 1.931923388228935888E-17, -0.04534722222222122012 ) ) ;
#23239 = CARTESIAN_POINT ( 'NONE',  ( -0.3850752722190822763, -0.3189425652913190912, 0.07813238993955241851 ) ) ;
#23240 = EDGE_CURVE ( 'NONE', #18019, #16762, #17333, .T. ) ;
#23241 = CARTESIAN_POINT ( 'NONE',  ( -0.2233192592356399442, 0.2330357141881718441, -0.3073725909049500049 ) ) ;
#23242 = CARTESIAN_POINT ( 'NONE',  ( 0.2819296736111110979, 0.5909722221463555858, 0.000000000000000000 ) ) ;
#23243 = CARTESIAN_POINT ( 'NONE',  ( 0.2764156081756484196, -5.077672346800151106E-17, 0.01194444444444569750 ) ) ;
#23244 = DIRECTION ( 'NONE',  ( -0.000000000000000000, -1.000000000000000000, -0.000000000000000000 ) ) ;
#23245 = CARTESIAN_POINT ( 'NONE',  ( -0.1219426170922269514, -0.2560469716179860633, -0.07222464464025338260 ) ) ;
#23246 = CARTESIAN_POINT ( 'NONE',  ( 0.000000000000000000, 0.2764156081756484196, 0.4147222222222267107 ) ) ;
#23247 = ORIENTED_EDGE ( 'NONE', *, *, #7063, .T. ) ;
#23248 = CARTESIAN_POINT ( 'NONE',  ( 0.6211549996190571798, 7.721695522547942866E-17, -0.1199999999999999956 ) ) ;
#23249 = CARTESIAN_POINT ( 'NONE',  ( -0.2805582969777798974, 4.275873129557496100, -0.1383904727280197144 ) ) ;
#23250 = CARTESIAN_POINT ( 'NONE',  ( 2.986000000000000210, 0.05000000000000024564, -2.541000000000000369 ) ) ;
#23251 = CARTESIAN_POINT ( 'NONE',  ( -0.3119999999999999996, 0.4381944444444440534, 0.1292346314604056190 ) ) ;
#23252 = CARTESIAN_POINT ( 'NONE',  ( -1.910449006669871087E-17, 5.036888888888888971, -0.3119999999999999996 ) ) ;
#23253 = APPROVAL ( #20977, 'UNKNOWN' ) ;
#23254 = CARTESIAN_POINT ( 'NONE',  ( 0.2819296736111111534, 4.210500000075865223, 0.1167790944451422563 ) ) ;
#23255 = EDGE_CURVE ( 'NONE', #20423, #9842, #4399, .T. ) ;
#23256 = CARTESIAN_POINT ( 'NONE',  ( 0.1167790944451422702, 3.960500000075866556, -0.2819296736111110424 ) ) ;
#23257 = CARTESIAN_POINT ( 'NONE',  ( 0.3860879860166684940, 4.111524471938507119, -2.831872695974971599 ) ) ;
#23258 = DIRECTION ( 'NONE',  ( -0.000000000000000000, -1.000000000000000000, -0.000000000000000000 ) ) ;
#23259 = LINE ( 'NONE', #2561, #516 ) ;
#23260 = ORIENTED_EDGE ( 'NONE', *, *, #1036, .T. ) ;
#23261 = VERTEX_POINT ( 'NONE', #10029 ) ;
#23262 = DIRECTION ( 'NONE',  ( -0.000000000000000000, 0.9767851838303062140, -0.2142211582677939208 ) ) ;
#23263 = CARTESIAN_POINT ( 'NONE',  ( -1.726321361862525858E-17, 4.616750000075865223, -0.2819296736111110979 ) ) ;
#23264 = CARTESIAN_POINT ( 'NONE',  ( -0.1292346314604057300, 4.116749999999998799, 0.3119999999999998885 ) ) ;
#23265 = AXIS2_PLACEMENT_3D ( 'NONE', #23257, #17789, #4618 ) ;
#23266 = PERSON_AND_ORGANIZATION_ROLE ( 'classification_officer' ) ;
#23267 = CARTESIAN_POINT ( 'NONE',  ( -0.4687500000000003886, 0.1743516731584483781, 0.07807856808314557473 ) ) ;
#23268 = CARTESIAN_POINT ( 'NONE',  ( 0.000000000000000000, 0.2764156081756484196, -0.03666666666666578561 ) ) ;
#23269 = CARTESIAN_POINT ( 'NONE',  ( -0.2819296736111110424, 3.981333333409199593, 0.1167790944451424923 ) ) ;
#23270 = CARTESIAN_POINT ( 'NONE',  ( -0.07900779940945044932, 4.823921452132610810, -0.3024882769266306615 ) ) ;
#23271 = CARTESIAN_POINT ( 'NONE',  ( -0.3119999999999999996, 4.880638888888888083, -0.1292346314604056468 ) ) ;
#23272 = CARTESIAN_POINT ( 'NONE',  ( -0.2764156081756484196, 0.1144950937579609918, 0.2584722222222254340 ) ) ;
#23273 = CARTESIAN_POINT ( 'NONE',  ( 0.1116596296178199027, 0.1401785713310290116, 0.3436530038418508792 ) ) ;
#23274 = CARTESIAN_POINT ( 'NONE',  ( -0.1167790944451424368, 0.5874999999241333759, 0.2819296736111110424 ) ) ;
#23275 = CARTESIAN_POINT ( 'NONE',  ( -0.04643634559190771421, 0.5144558407376040865, 0.07050986311825922781 ) ) ;
#23276 = DIRECTION ( 'NONE',  ( 0.000000000000000000, -0.7071067811865474617, 0.7071067811865476838 ) ) ;
#23277 = CARTESIAN_POINT ( 'NONE',  ( -0.3155070326520293400, -0.1306872919485614626, 0.3435416666666703533 ) ) ;
#23278 = VERTEX_POINT ( 'NONE', #6833 ) ;
#23279 = CARTESIAN_POINT ( 'NONE',  ( 0.3119999999999999996, 3.967444444444443441, -3.820898013339742174E-17 ) ) ;
#23280 = CARTESIAN_POINT ( 'NONE',  ( -0.3038822597986416407, 3.782168817998234456, 0.08165548423408781897 ) ) ;
#23281 = CARTESIAN_POINT ( 'NONE',  ( 0.2209708691207961095, -0.2209708691207961651, 0.02583333333333451623 ) ) ;
#23282 = CARTESIAN_POINT ( 'NONE',  ( 0.1993543840281266910, 0.4868055554796889561, -0.1993543840281266910 ) ) ;
#23283 = CARTESIAN_POINT ( 'NONE',  ( -0.2819296736111110424, 4.029944444520309865, -0.1167790944451423119 ) ) ;
#23284 = TOROIDAL_SURFACE ( 'NONE', #20569, 0.2510000000000000009, 0.0009999999999999859262 ) ;
#23285 = CARTESIAN_POINT ( 'NONE',  ( 0.1236067977499789028, 0.4482142855192008946, 0.3804226065180614791 ) ) ;
#23286 = EDGE_CURVE ( 'NONE', #8318, #11169, #16189, .T. ) ;
#23287 = CARTESIAN_POINT ( 'NONE',  ( 0.1993543840281266633, 4.623694444520309865, -0.1993543840281266910 ) ) ;
#23288 = CARTESIAN_POINT ( 'NONE',  ( 0.3065460696617670067, 5.130431554589877763, 0.02195525653071019045 ) ) ;
#23289 = CARTESIAN_POINT ( 'NONE',  ( 0.2637416282169243176, 5.083478233281141456, -0.1669753523072903256 ) ) ;
#23290 = ORIENTED_EDGE ( 'NONE', *, *, #15440, .F. ) ;
#23291 = CARTESIAN_POINT ( 'NONE',  ( 0.3119999999999999996, 4.800777777777776478, -3.820898013339742174E-17 ) ) ;
#23292 = CARTESIAN_POINT ( 'NONE',  ( -0.3119999999999999996, 3.946611111262843252, 0.000000000000000000 ) ) ;
#23293 = DIRECTION ( 'NONE',  ( -0.000000000000000000, -1.000000000000000000, -0.000000000000000000 ) ) ;
#23294 = DIRECTION ( 'NONE',  ( 1.000000000000000000, 0.000000000000000000, 0.000000000000000000 ) ) ;
#23295 = CARTESIAN_POINT ( 'NONE',  ( 0.2550676506477509431, 0.03242967361111052244, 0.1209729261660745098 ) ) ;
#23296 = AXIS2_PLACEMENT_3D ( 'NONE', #22244, #11041, #7262 ) ;
#23297 = CARTESIAN_POINT ( 'NONE',  ( -0.2819296736111110979, 4.797305555631420582, 0.000000000000000000 ) ) ;
#23298 = APPLICATION_PROTOCOL_DEFINITION ( 'international standard', 'config_control_design', 1994, #18859 ) ;
#23299 = ORIENTED_EDGE ( 'NONE', *, *, #14552, .F. ) ;
#23300 = CARTESIAN_POINT ( 'NONE',  ( -0.2681623976265802289, 5.109836857663620613, -0.1564668307319910245 ) ) ;
#23301 = EDGE_CURVE ( 'NONE', #15146, #15771, #1221, .T. ) ;
#23302 = CARTESIAN_POINT ( 'NONE',  ( -0.2064849667589426785, 4.565315176446661738, 0.2372659973544750944 ) ) ;
#23303 = ORIENTED_EDGE ( 'NONE', *, *, #23714, .T. ) ;
#23304 = CARTESIAN_POINT ( 'NONE',  ( 0.1993543840281266355, 0.04236111103524448085, 0.1993543840281267465 ) ) ;
#23305 = EDGE_CURVE ( 'NONE', #3503, #23698, #3717, .T. ) ;
#23306 = EDGE_CURVE ( 'NONE', #23447, #7051, #12042, .T. ) ;
#23307 = ORIENTED_EDGE ( 'NONE', *, *, #13462, .F. ) ;
#23308 = FACE_OUTER_BOUND ( 'NONE', #4907, .T. ) ;
#23309 = DIRECTION ( 'NONE',  ( 1.000000000000000000, 0.000000000000000000, 6.123233995736811642E-17 ) ) ;
#23310 = CARTESIAN_POINT ( 'NONE',  ( -0.5116234456863466562, 1.808198851485059988, 2.664840263418369659 ) ) ;
#23311 = CARTESIAN_POINT ( 'NONE',  ( 0.3613381517857143232, 0.2116071427596004084, -0.1174058825155740587 ) ) ;
#23312 = CARTESIAN_POINT ( 'NONE',  ( -0.2578690707795402992, 5.052376359289721286, -0.1763080320115959498 ) ) ;
#23313 = DIRECTION ( 'NONE',  ( 0.000000000000000000, 1.000000000000000000, 0.000000000000000000 ) ) ;
#23314 = DIMENSIONAL_EXPONENTS ( 1.000000000000000000, 0.000000000000000000, 0.000000000000000000, 0.000000000000000000, 0.000000000000000000, 0.000000000000000000, 0.000000000000000000 ) ;
#23315 = CARTESIAN_POINT ( 'NONE',  ( 0.000000000000000000, 0.000000000000000000, 1.326383476483184332 ) ) ;
#23316 = ADVANCED_FACE ( 'NONE', ( #4939 ), #3231, .T. ) ;
#23317 = CARTESIAN_POINT ( 'NONE',  ( -0.2819296736111110979, 3.797305555631421470, 0.000000000000000000 ) ) ;
#23318 = CARTESIAN_POINT ( 'NONE',  ( 0.09843671724995897709, 5.018886197857182374, 0.2967729835320978005 ) ) ;
#23319 = CARTESIAN_POINT ( 'NONE',  ( 0.09694982473845883963, 0.06249891840240667101, 0.2965547697865978938 ) ) ;
#23320 = FACE_OUTER_BOUND ( 'NONE', #3802, .T. ) ;
#23321 = CARTESIAN_POINT ( 'NONE',  ( -0.3119999999999998885, 4.561194444596177178, 0.1292346314604058410 ) ) ;
#23322 = CARTESIAN_POINT ( 'NONE',  ( -0.1993543840281266355, 4.707027777853643791, 0.1993543840281267465 ) ) ;
#23323 = ORIENTED_EDGE ( 'NONE', *, *, #7809, .F. ) ;
#23324 = CARTESIAN_POINT ( 'NONE',  ( -0.1167790944451423535, 4.085500000075865223, 0.2819296736111110424 ) ) ;
#23325 = PRODUCT ( 'MAS-409', 'MAS-409', '', ( #969 ) ) ;
#23326 = VERTEX_POINT ( 'NONE', #6771 ) ;
#23327 = PERSON_AND_ORGANIZATION_ROLE ( 'creator' ) ;
#23328 = CARTESIAN_POINT ( 'NONE',  ( 0.3124999999999999445, 0.1294417382415923023, 0.04319444444444614506 ) ) ;
#23329 = CARTESIAN_POINT ( 'NONE',  ( 0.9244709581221671746, 2.291712385858714729, -1.333428253224822280 ) ) ;
#23330 = CARTESIAN_POINT ( 'NONE',  ( 0.1292346314604056745, 0.02152777762604484585, -0.3119999999999999996 ) ) ;
#23331 = CIRCLE ( 'NONE', #16341, 0.3125000000000000000 ) ;
#23332 = CARTESIAN_POINT ( 'NONE',  ( -0.3039450333671691595, 4.388825253606679411, -0.08146239154257989279 ) ) ;
#23333 = CARTESIAN_POINT ( 'NONE',  ( 0.000000000000000000, 5.384999999999999787, -0.3119999999999999996 ) ) ;
#23334 = FACE_OUTER_BOUND ( 'NONE', #2629, .T. ) ;
#23335 = EDGE_LOOP ( 'NONE', ( #6035, #15006 ) ) ;
#23336 = DIRECTION ( 'NONE',  ( -1.000000000000000000, 0.000000000000000000, 0.000000000000000000 ) ) ;
#23337 = DIRECTION ( 'NONE',  ( 0.000000000000000000, 1.000000000000000000, 0.000000000000000000 ) ) ;
#23338 = CARTESIAN_POINT ( 'NONE',  ( 0.2764156081756484196, -5.077672346800151106E-17, 0.1161111111111132049 ) ) ;
#23339 = ORIENTED_EDGE ( 'NONE', *, *, #17335, .F. ) ;
#23340 = CYLINDRICAL_SURFACE ( 'NONE', #13995, 0.3119999999999999996 ) ;
#23341 = ADVANCED_FACE ( 'NONE', ( #1290 ), #9579, .F. ) ;
#23342 = CARTESIAN_POINT ( 'NONE',  ( 0.1993543840281267465, 4.484805555631420582, 0.1993543840281266633 ) ) ;
#23343 = DIRECTION ( 'NONE',  ( -0.000000000000000000, -1.000000000000000000, -0.000000000000000000 ) ) ;
#23344 = CARTESIAN_POINT ( 'NONE',  ( -0.2829524303836037369, 0.6104264140268672589, -1.091612836571470568 ) ) ;
#23345 = DIRECTION ( 'NONE',  ( 0.000000000000000000, 0.000000000000000000, -1.000000000000000000 ) ) ;
#23346 = DIRECTION ( 'NONE',  ( 0.000000000000000000, 0.9659258262890680902, 0.2588190451025214611 ) ) ;
#23347 = CARTESIAN_POINT ( 'NONE',  ( 0.3119999999999999996, 4.300777777777777366, -3.820898013339742174E-17 ) ) ;
#23348 = CARTESIAN_POINT ( 'NONE',  ( -0.3119999999999999996, 4.658416666666666650, -0.1292346314604056468 ) ) ;
#23349 = CIRCLE ( 'NONE', #12881, 0.2109499999999998043 ) ;
#23350 = ADVANCED_BREP_SHAPE_REPRESENTATION ( '', ( #1082, #9127 ), #7955 ) ;
#23351 = TOROIDAL_SURFACE ( 'NONE', #2358, 0.6211549996190571798, 0.01874999999999999931 ) ;
#23352 = CARTESIAN_POINT ( 'NONE',  ( 2.108637995767629114, 2.978485840173427324, -1.763529041877836434 ) ) ;
#23353 = EDGE_LOOP ( 'NONE', ( #11517, #5495, #11609, #11956 ) ) ;
#23354 = CARTESIAN_POINT ( 'NONE',  ( -0.1916180747362854764, 4.899256411840736014, 0.2495837949844624815 ) ) ;
#23355 = APPLICATION_CONTEXT ( 'configuration controlled 3d designs of mechanical parts and assemblies' ) ;
#23356 = UNCERTAINTY_MEASURE_WITH_UNIT (LENGTH_MEASURE( 1.000000000000000082E-05 ), #17469, 'distance_accuracy_value', 'NONE');
#23357 = LINE ( 'NONE', #6428, #9614 ) ;
#23358 = CARTESIAN_POINT ( 'NONE',  ( 0.3155070326520292290, -0.1306872919485616569, 0.09006944444444651976 ) ) ;
#23359 = DIRECTION ( 'NONE',  ( 0.000000000000000000, 1.000000000000000000, 0.000000000000000000 ) ) ;
#23360 = CARTESIAN_POINT ( 'NONE',  ( 0.08166450070216819956, 3.796057964755177760, 0.3038796990105872564 ) ) ;
#23361 = VERTEX_POINT ( 'NONE', #8349 ) ;
#23362 = AXIS2_PLACEMENT_3D ( 'NONE', #2434, #11958, #13774 ) ;
#23363 = CARTESIAN_POINT ( 'NONE',  ( -0.3613381517857143232, 0.1687499999024575370, -0.1174058825155741004 ) ) ;
#23364 = AXIS2_PLACEMENT_3D ( 'NONE', #8412, #8537, #23400 ) ;
#23365 = FACE_OUTER_BOUND ( 'NONE', #16649, .T. ) ;
#23366 = CARTESIAN_POINT ( 'NONE',  ( -0.2764156081756484196, 1.692557448933383907E-17, 0.09527777777777970969 ) ) ;
#23367 = DIRECTION ( 'NONE',  ( 0.000000000000000000, 0.000000000000000000, -1.000000000000000000 ) ) ;
#23368 = CARTESIAN_POINT ( 'NONE',  ( -0.1993543840281266355, 5.095916666742533074, 0.1993543840281267465 ) ) ;
#23369 = CARTESIAN_POINT ( 'NONE',  ( 0.000000000000000000, 0.02999999999999995379, 0.000000000000000000 ) ) ;
#23370 = ORIENTED_EDGE ( 'NONE', *, *, #14595, .T. ) ;
#23371 = EDGE_CURVE ( 'NONE', #8265, #19443, #8231, .T. ) ;
#23372 = CARTESIAN_POINT ( 'NONE',  ( -0.2507716889269062666, 4.607602545532474281, -0.1880287605004705154 ) ) ;
#23373 = CARTESIAN_POINT ( 'NONE',  ( -0.3103924686884816375, 4.278734377591210780, -0.04199753653605552139 ) ) ;
#23374 = CARTESIAN_POINT ( 'NONE',  ( -0.4587689423274134426, -0.1777187644174526848, 0.4166100394118468220 ) ) ;
#23375 = CARTESIAN_POINT ( 'NONE',  ( 0.3119999999999999996, 0.5180555555555551583, 0.000000000000000000 ) ) ;
#23376 = CARTESIAN_POINT ( 'NONE',  ( -0.2206173157302027676, 4.891055555555555046, 0.2206173157302028787 ) ) ;
#23377 = CARTESIAN_POINT ( 'NONE',  ( 5.178964085587577574E-17, 4.311194444520309865, 0.2819296736111110979 ) ) ;
#23378 = CARTESIAN_POINT ( 'NONE',  ( -0.1167790944451423535, 3.988277777853643347, 0.2819296736111110424 ) ) ;
#23379 = CARTESIAN_POINT ( 'NONE',  ( -0.3075813148943709052, 0.3526675668868786695, 0.4297318021117937925 ) ) ;
#23380 = CARTESIAN_POINT ( 'NONE',  ( 0.4687500000000002776, 0.2598076211353318454, 0.4425000000000000044 ) ) ;
#23381 = ORIENTED_EDGE ( 'NONE', *, *, #6647, .F. ) ;
#23382 = LINE ( 'NONE', #17916, #9733 ) ;
#23383 = CARTESIAN_POINT ( 'NONE',  ( -0.2819296736111110424, 4.404944444520309865, -0.1167790944451423119 ) ) ;
#23384 = DIRECTION ( 'NONE',  ( 0.000000000000000000, 0.000000000000000000, -1.000000000000000000 ) ) ;
#23385 = LINE ( 'NONE', #4861, #2149 ) ;
#23386 = AXIS2_PLACEMENT_3D ( 'NONE', #2322, #3697, #9063 ) ;
#23387 = DATE_TIME_ROLE ( 'creation_date' ) ;
#23388 = CARTESIAN_POINT ( 'NONE',  ( -0.4800179949082463149, -0.1716548275489190312, 0.06108632444355151930 ) ) ;
#23389 = CARTESIAN_POINT ( 'NONE',  ( 0.2764156081756483641, 0.1144950937579610056, 0.06402777777777945989 ) ) ;
#23390 = DIRECTION ( 'NONE',  ( -0.5773502691896257311, 0.5773502691896257311, 0.5773502691896257311 ) ) ;
#23391 = CARTESIAN_POINT ( 'NONE',  ( -0.1167790944451423535, 4.154944444520310753, 0.2819296736111110979 ) ) ;
#23392 = PERSON_AND_ORGANIZATION_ROLE ( 'classification_officer' ) ;
#23393 = DIRECTION ( 'NONE',  ( 0.8660254037844434816, 2.725147086360870403E-18, -0.4999999999999913403 ) ) ;
#23394 = APPROVAL ( #22802, 'UNSPECIFIED' ) ;
#23395 = CARTESIAN_POINT ( 'NONE',  ( -0.1144950937579609918, -0.2764156081756484196, 0.1056944444444464365 ) ) ;
#23396 = CARTESIAN_POINT ( 'NONE',  ( 0.1116596296178199860, 0.02589285704531473636, -0.3436530038418508792 ) ) ;
#23397 = CARTESIAN_POINT ( 'NONE',  ( -5.178964085587577574E-17, 0.5909722221463555858, 0.2819296736111110979 ) ) ;
#23398 = CARTESIAN_POINT ( 'NONE',  ( -0.1595362993632639947, 0.2449369388610319331, 0.4038266169345403611 ) ) ;
#23399 = CARTESIAN_POINT ( 'NONE',  ( -0.1292346314604056190, 0.09097222222222188515, -0.3119999999999999996 ) ) ;
#23400 = DIRECTION ( 'NONE',  ( 0.8660254037844526964, 0.000000000000000000, 0.4999999999999757416 ) ) ;
#23401 = CARTESIAN_POINT ( 'NONE',  ( 0.000000000000000000, 3.575000000000000622, 0.000000000000000000 ) ) ;
#23402 = CARTESIAN_POINT ( 'NONE',  ( -0.2230971623002953874, 0.2230971623002954152, 0.2775694444444475883 ) ) ;
#23403 = ORIENTED_EDGE ( 'NONE', *, *, #1428, .T. ) ;
#23404 = DIRECTION ( 'NONE',  ( 0.8660254037844434816, 0.000000000000000000, -0.4999999999999916178 ) ) ;
#23405 = CARTESIAN_POINT ( 'NONE',  ( -0.004454008101752859362, 3.766175329530188076, -0.3119727745386958184 ) ) ;
#23406 = LINE ( 'NONE', #21589, #21034 ) ;
#23407 = CARTESIAN_POINT ( 'NONE',  ( -5.178964085587577574E-17, 0.3548611110352444808, 0.2819296736111110979 ) ) ;
#23408 = CARTESIAN_POINT ( 'NONE',  ( 0.1993543840281266633, 4.012583333409199149, -0.1993543840281266910 ) ) ;
#23409 = CARTESIAN_POINT ( 'NONE',  ( -0.2472135954999579999, 0.4374999998049151628, 0.3402603233408159622 ) ) ;
#23410 = VERTEX_POINT ( 'NONE', #21289 ) ;
#23411 = CARTESIAN_POINT ( 'NONE',  ( 0.1993543840281267465, 4.665361111186976828, 0.1993543840281266633 ) ) ;
#23412 = CARTESIAN_POINT ( 'NONE',  ( 0.2020813919255678437, 5.124140614773011748, 0.2323642223043996258 ) ) ;
#23413 = CARTESIAN_POINT ( 'NONE',  ( 0.2472135954999579721, 0.1874999998049151628, -0.3402603233408160732 ) ) ;
#23414 = ORIENTED_EDGE ( 'NONE', *, *, #23894, .T. ) ;
#23415 = CARTESIAN_POINT ( 'NONE',  ( 0.3120000000000000551, 4.797305555555555046, 0.1292346314604056190 ) ) ;
#23416 = CARTESIAN_POINT ( 'NONE',  ( 0.1167790944451424368, 5.092444444520309865, 0.2819296736111110424 ) ) ;
#23417 = CARTESIAN_POINT ( 'NONE',  ( 0.2664282082089008408, 4.191741270665894525, 0.1623755266555968191 ) ) ;
#23418 = EDGE_CURVE ( 'NONE', #23057, #1943, #14096, .T. ) ;
#23419 = ORIENTED_EDGE ( 'NONE', *, *, #21045, .T. ) ;
#23420 = CARTESIAN_POINT ( 'NONE',  ( 0.2819296736111110979, 4.936194444520309865, -3.452642723725051716E-17 ) ) ;
#23421 = APPROVAL_ROLE ( '' ) ;
#23422 = ORIENTED_EDGE ( 'NONE', *, *, #666, .T. ) ;
#23423 = EDGE_CURVE ( 'NONE', #1686, #11401, #12715, .T. ) ;
#23424 = CARTESIAN_POINT ( 'NONE',  ( -0.3066395854341782967, 5.113642974739954106, -0.04204093653351399090 ) ) ;
#23425 = CARTESIAN_POINT ( 'NONE',  ( 2.802071455580988509E-07, 4.599388881221821990, -0.3119999999998741003 ) ) ;
#23426 = VERTEX_POINT ( 'NONE', #19455 ) ;
#23427 = CARTESIAN_POINT ( 'NONE',  ( 0.1167790944451423257, 0.3930555554796889561, -0.2819296736111110424 ) ) ;
#23428 = ORIENTED_EDGE ( 'NONE', *, *, #8157, .T. ) ;
#23429 = CARTESIAN_POINT ( 'NONE',  ( 0.000000000000000000, 5.500232050807569273, 0.000000000000000000 ) ) ;
#23430 = CARTESIAN_POINT ( 'NONE',  ( 1.864417095468034626E-17, 0.5918402777588108732, -0.3044824184027777880 ) ) ;
#23431 = CARTESIAN_POINT ( 'NONE',  ( -0.5116234456863466562, 4.027014562472920112, 2.739895798413020778 ) ) ;
#23432 = CARTESIAN_POINT ( 'NONE',  ( 0.2923287055106771337, 0.2151785713310289949, -0.2123892367102620249 ) ) ;
#23433 = CARTESIAN_POINT ( 'NONE',  ( -6.528214817076446933E-07, 5.071585437816050757, 0.3119999999985565986 ) ) ;
#23434 = LINE ( 'NONE', #12255, #10041 ) ;
#23435 = CARTESIAN_POINT ( 'NONE',  ( -1.726321361862525858E-17, 4.630638888964754507, -0.2819296736111110979 ) ) ;
#23436 = CARTESIAN_POINT ( 'NONE',  ( -0.1566809303765275552, 4.659511855693362570, -0.2728735228218804321 ) ) ;
#23437 = CARTESIAN_POINT ( 'NONE',  ( -0.1167790944451423535, 3.863277777853643791, 0.2819296736111110424 ) ) ;
#23438 = DIRECTION ( 'NONE',  ( 0.000000000000000000, 1.000000000000000000, 0.000000000000000000 ) ) ;
#23439 = CARTESIAN_POINT ( 'NONE',  ( 0.2485560646891840364, 5.024144980645338876, 0.1929866496405842624 ) ) ;
#23440 = DIRECTION ( 'NONE',  ( -0.000000000000000000, -0.9961946980917454342, 0.08715574274765830465 ) ) ;
#23441 = CARTESIAN_POINT ( 'NONE',  ( -0.1292346314604056745, 4.213972222373954857, -0.3119999999999999996 ) ) ;
#23442 = CARTESIAN_POINT ( 'NONE',  ( 5.178964085587577574E-17, 4.713972222298088433, 0.2819296736111110979 ) ) ;
#23443 = EDGE_CURVE ( 'NONE', #20947, #16517, #2753, .T. ) ;
#23444 = VERTEX_POINT ( 'NONE', #8606 ) ;
#23445 = CARTESIAN_POINT ( 'NONE',  ( 0.2819296736111110979, 4.099388888964754507, 0.1167790944451422425 ) ) ;
#23446 = ADVANCED_FACE ( 'NONE', ( #14337 ), #12164, .T. ) ;
#23447 = VERTEX_POINT ( 'NONE', #21769 ) ;
#23448 = VECTOR ( 'NONE', #1797, 39.37007874015747433 ) ;
#23449 = VERTEX_POINT ( 'NONE', #5056 ) ;
#23450 = PERSON_AND_ORGANIZATION ( #15518, #2538 ) ;
#23451 = ADVANCED_FACE ( 'NONE', ( #803 ), #919, .T. ) ;
#23452 = CARTESIAN_POINT ( 'NONE',  ( 0.000000000000000000, 0.3125000000000000000, 0.05361111111111287880 ) ) ;
#23453 = FACE_BOUND ( 'NONE', #13715, .T. ) ;
#23454 = VERTEX_POINT ( 'NONE', #19572 ) ;
#23455 = CARTESIAN_POINT ( 'NONE',  ( -0.1292346314604058410, 0.2159722220704893003, 0.3119999999999998885 ) ) ;
#23456 = CARTESIAN_POINT ( 'NONE',  ( -0.01598815013341712762, 4.377598596822689814, -0.3116164386091518912 ) ) ;
#23457 = CARTESIAN_POINT ( 'NONE',  ( -0.4687500000000003886, -0.2178027435389952027, 0.3900764204055337525 ) ) ;
#23458 = CARTESIAN_POINT ( 'NONE',  ( -1.861236469537744314E-17, 5.143359825938298435, -0.3039629827691722741 ) ) ;
#23459 = ORIENTED_EDGE ( 'NONE', *, *, #16976, .F. ) ;
#23460 = CARTESIAN_POINT ( 'NONE',  ( 1.910449006669871087E-17, 0.2472222220704892726, -0.3119999999999999996 ) ) ;
#23461 = CARTESIAN_POINT ( 'NONE',  ( 0.1167790944451423535, 0.08055555547968892838, 0.2819296736111110979 ) ) ;
#23462 = CARTESIAN_POINT ( 'NONE',  ( -0.1144950937579609918, -0.2764156081756484196, -0.01236111111111004406 ) ) ;
#23463 = ORIENTED_EDGE ( 'NONE', *, *, #4520, .T. ) ;
#23464 = CIRCLE ( 'NONE', #16089, 0.09499999999999995948 ) ;
#23465 = CARTESIAN_POINT ( 'NONE',  ( 0.2819296736111110424, 4.439666666742532186, -0.1167790944451423396 ) ) ;
#23466 = CARTESIAN_POINT ( 'NONE',  ( 0.000000000000000000, 5.384999999999999787, 0.000000000000000000 ) ) ;
#23467 = CARTESIAN_POINT ( 'NONE',  ( -0.2079132705422924166, 0.7081134582484001072, -1.081719846782932759 ) ) ;
#23468 = CARTESIAN_POINT ( 'NONE',  ( -0.3125000000000000000, 1.913510623667739771E-17, -0.05055555555555497210 ) ) ;
#23469 = FACE_OUTER_BOUND ( 'NONE', #5386, .T. ) ;
#23470 = CARTESIAN_POINT ( 'NONE',  ( 5.731347020009612645E-17, 3.953555555555555046, 0.3119999999999999996 ) ) ;
#23471 = CARTESIAN_POINT ( 'NONE',  ( -1.910449006669871087E-17, 5.154944444596176290, -0.3119999999999999996 ) ) ;
#23472 = CARTESIAN_POINT ( 'NONE',  ( 0.3117034358253052972, 4.973992755114602815, 0.01468513461878798859 ) ) ;
#23473 = DIRECTION ( 'NONE',  ( 0.000000000000000000, 0.9659258262890680902, 0.2588190451025215166 ) ) ;
#23474 = ORIENTED_EDGE ( 'NONE', *, *, #5129, .T. ) ;
#23475 = CARTESIAN_POINT ( 'NONE',  ( 0.1294417382415924134, 0.3124999999999999445, 0.2168055555555586100 ) ) ;
#23476 = AXIS2_PLACEMENT_3D ( 'NONE', #4515, #19152, #13572 ) ;
#23477 = CARTESIAN_POINT ( 'NONE',  ( -0.3155070326520293400, 0.1306872919485614903, 0.1178472222222245319 ) ) ;
#23478 = CARTESIAN_POINT ( 'NONE',  ( 0.1116596296178199027, 0.3544642856167432576, 0.3436530038418508792 ) ) ;
#23479 = CARTESIAN_POINT ( 'NONE',  ( 0.03651601414450977162, -0.2739930093161348501, 0.3880822748423153890 ) ) ;
#23480 = ORIENTED_EDGE ( 'NONE', *, *, #8425, .T. ) ;
#23481 = CARTESIAN_POINT ( 'NONE',  ( -0.2923287055106771337, 0.2508928570453147211, 0.2123892367102619971 ) ) ;
#23482 = PLANE ( 'NONE',  #22604 ) ;
#23483 = CARTESIAN_POINT ( 'NONE',  ( -0.1144950937579609779, 0.2764156081756484196, -0.02624999999999906228 ) ) ;
#23484 = CARTESIAN_POINT ( 'NONE',  ( 0.4772460259542070649, -0.2717629240624622744, 0.04193793378272828165 ) ) ;
#23485 = CARTESIAN_POINT ( 'NONE',  ( 0.1167790944451422702, 5.071611111186976828, -0.2819296736111110424 ) ) ;
#23486 = DIRECTION ( 'NONE',  ( -0.000000000000000000, -1.000000000000000000, -0.000000000000000000 ) ) ;
#23487 = ORIENTED_EDGE ( 'NONE', *, *, #17528, .F. ) ;
#23488 = CARTESIAN_POINT ( 'NONE',  ( -0.04004678673780891901, 4.600547297044312423, -0.3095819090388297057 ) ) ;
#23489 = CARTESIAN_POINT ( 'NONE',  ( 0.3236067977499789694, 0.1071428571428571092, 0.2351141009169893659 ) ) ;
#23490 = FACE_BOUND ( 'NONE', #9816, .T. ) ;
#23491 = CARTESIAN_POINT ( 'NONE',  ( 0.1292346314604056745, 0.5284722222222218990, -0.3119999999999999996 ) ) ;
#23492 = CARTESIAN_POINT ( 'NONE',  ( -0.3119999999999999996, 4.713972222222221120, -0.1292346314604056468 ) ) ;
#23493 = CARTESIAN_POINT ( 'NONE',  ( -0.1167790944451423535, 4.141055555631421470, 0.2819296736111110979 ) ) ;
#23494 = AXIS2_PLACEMENT_3D ( 'NONE', #2466, #4526, #19401 ) ;
#23495 = CARTESIAN_POINT ( 'NONE',  ( 0.2819296736111110979, 3.835500000075866556, 0.1167790944451422425 ) ) ;
#23496 = CARTESIAN_POINT ( 'NONE',  ( 0.000000000000000000, 0.4987679491924311148, 0.2500000000000000000 ) ) ;
#23497 = CARTESIAN_POINT ( 'NONE',  ( -0.3267728913538784918, 0.3414772273308728789, 0.4269974078869069323 ) ) ;
#23498 = ORIENTED_EDGE ( 'NONE', *, *, #5798, .F. ) ;
#23499 = CARTESIAN_POINT ( 'NONE',  ( -0.1294417382415922191, 0.3125000000000000000, 0.1126388888888911199 ) ) ;
#23500 = CARTESIAN_POINT ( 'NONE',  ( 0.2819296736111110979, 4.436194444520309865, -3.452642723725051716E-17 ) ) ;
#23501 = CARTESIAN_POINT ( 'NONE',  ( 0.1986479633932748956, -0.2391244849433121489, 0.4220858545751106639 ) ) ;
#23502 = B_SPLINE_CURVE_WITH_KNOTS ( 'NONE', 3,
 ( #9207, #12890, #16648, #2727, #8325, #11766, #17128, #11524, #417, #4310, #13832, #8206, #10181, #22847, #11896, #22726, #19187, #18957, #6136, #2255, #17482, #17604, #894, #11646, #17248, #10058, #532, #19071, #15777, #21016, #19311, #7850, #7968, #15655, #774, #15299, #13484, #2496, #9935, #15419, #13603, #17364, #656, #9689, #20779, #8084 ),
 .UNSPECIFIED., .F., .F.,
 ( 4, 2, 2, 2, 2, 2, 2, 2, 2, 2, 2, 2, 2, 2, 2, 2, 2, 2, 2, 2, 2, 2, 4 ),
 ( 0.09082637236171775541, 0.09155946950567490916, 0.09229256664963206291, 0.09375876093754638430, 0.09522495522546070568, 0.09595805236941785943, 0.09669114951337501318, 0.09815734380128933456, 0.09962353808920364207, 0.1010897323771179634, 0.1018228295210751172, 0.1025559266650322848, 0.1032890238089894386, 0.1040221209529466062, 0.1054883152408609276, 0.1069545095287752490, 0.1084207038166895565, 0.1091538009606467241, 0.1098868981046038779, 0.1113530923925181854, 0.1128192866804325067, 0.1135523838243896605, 0.1142854809683468142 ),
 .UNSPECIFIED. ) ;
#23503 = CARTESIAN_POINT ( 'NONE',  ( 0.4679361169221505912, -0.2662350510444111418, 0.05893285591566548021 ) ) ;
#23504 = EDGE_CURVE ( 'NONE', #23426, #18391, #10346, .T. ) ;
#23505 = APPROVAL_DATE_TIME ( #18158, #19972 ) ;
#23506 = CARTESIAN_POINT ( 'NONE',  ( -0.4620753182980354978, -0.2744865679600219099, 0.05975678175779885332 ) ) ;
#23507 = CARTESIAN_POINT ( 'NONE',  ( -3.385114897866767815E-17, -0.2764156081756484196, 0.1022222222222241989 ) ) ;
#23508 = CARTESIAN_POINT ( 'NONE',  ( -0.2819296736111110979, 4.029944444520310753, -0.1167790944451422980 ) ) ;
#23509 = CARTESIAN_POINT ( 'NONE',  ( 0.5997114317030027841, 0.000000000000000000, -0.9454293994002404000 ) ) ;
#23510 = CYLINDRICAL_SURFACE ( 'NONE', #11298, 0.3119999999999999996 ) ;
#23511 = CARTESIAN_POINT ( 'NONE',  ( 0.1144950937579611444, 0.2764156081756483641, 0.1334722222222244348 ) ) ;
#23512 = CARTESIAN_POINT ( 'NONE',  ( -0.2923287055106771337, -0.01696428581182811424, 0.2123892367102619971 ) ) ;
#23513 = CARTESIAN_POINT ( 'NONE',  ( 0.2819296736111110979, -0.02013888896475552262, 0.000000000000000000 ) ) ;
#23514 = CARTESIAN_POINT ( 'NONE',  ( -0.1514593411830790493, 0.2498004213170096632, 0.4036436051450662532 ) ) ;
#23515 = PLANE ( 'NONE',  #19355 ) ;
#23516 = CARTESIAN_POINT ( 'NONE',  ( -0.2019078322727933528, 0.3016929934852337625, -0.7223299880601123935 ) ) ;
#23517 = CARTESIAN_POINT ( 'NONE',  ( -0.2764156081756484196, 0.1144950937579609918, -0.02624999999999903799 ) ) ;
#23518 = CARTESIAN_POINT ( 'NONE',  ( 0.2230971623002954429, 0.2230971623002953319, 0.3192361111111146066 ) ) ;
#23519 = ORIENTED_EDGE ( 'NONE', *, *, #7985, .T. ) ;
#23520 = CARTESIAN_POINT ( 'NONE',  ( 0.4620259694561523744, 0.2880908832651560281, 0.04413116910601654758 ) ) ;
#23521 = CARTESIAN_POINT ( 'NONE',  ( 1.337745543335387199E-07, 4.460505239618372642, 0.3119999999999396589 ) ) ;
#23522 = CARTESIAN_POINT ( 'NONE',  ( 0.1167790944451423535, 0.3583333332574666907, 0.2819296736111110424 ) ) ;
#23523 = CARTESIAN_POINT ( 'NONE',  ( -1.726321361862525858E-17, 3.908416666742532630, -0.2819296736111110979 ) ) ;
#23524 = CARTESIAN_POINT ( 'NONE',  ( -0.2923287055106771337, 0.05446428561674331731, 0.2123892367102619971 ) ) ;
#23525 = ORIENTED_EDGE ( 'NONE', *, *, #16789, .F. ) ;
#23526 = CARTESIAN_POINT ( 'NONE',  ( -0.1167790944451423535, 4.654944444520310753, 0.2819296736111110424 ) ) ;
#23527 = PRODUCT_DEFINITION_SHAPE ( 'NONE', 'NONE',  #8791 ) ;
#23528 = DIRECTION ( 'NONE',  ( -0.000000000000000000, -1.000000000000000000, -0.000000000000000000 ) ) ;
#23529 = CARTESIAN_POINT ( 'NONE',  ( 0.3119999999999998885, 0.3965277776260449083, 0.1292346314604058410 ) ) ;
#23530 = ORIENTED_EDGE ( 'NONE', *, *, #15276, .T. ) ;
#23531 = CARTESIAN_POINT ( 'NONE',  ( 0.3119999999999999996, 4.022999999999998799, -3.820898013339742174E-17 ) ) ;
#23532 = CARTESIAN_POINT ( 'NONE',  ( -0.1167790944451423535, 5.085500000075866112, 0.2819296736111110424 ) ) ;
#23533 = VECTOR ( 'NONE', #17384, 39.37007874015748143 ) ;
#23534 = CC_DESIGN_DATE_AND_TIME_ASSIGNMENT ( #5919, #19204, ( #6827 ) ) ;
#23535 = CARTESIAN_POINT ( 'NONE',  ( 0.2644034564220129058, 4.191631208498491468, 0.1656346508680236751 ) ) ;
#23536 = CARTESIAN_POINT ( 'NONE',  ( 0.1856355564575103978, 0.03242967361111056407, 0.2126852203547632825 ) ) ;
#23537 = CARTESIAN_POINT ( 'NONE',  ( 0.1179581865186765804, 5.206640035683670398, 0.2566525738614713892 ) ) ;
#23538 = AXIS2_PLACEMENT_3D ( 'NONE', #9770, #17205, #5619 ) ;
#23539 = CARTESIAN_POINT ( 'NONE',  ( -0.1993543840281266355, 4.915361111186976828, 0.1993543840281267465 ) ) ;
#23540 = SECURITY_CLASSIFICATION_LEVEL ( 'unclassified' ) ;
#23541 = ORIENTED_EDGE ( 'NONE', *, *, #2741, .F. ) ;
#23542 = CARTESIAN_POINT ( 'NONE',  ( -0.3091666942010690144, 5.114568388431837143, -0.01160475953834872766 ) ) ;
#23543 = CARTESIAN_POINT ( 'NONE',  ( -0.05196600641818320543, 4.570166421312822358, 0.3076424449429943642 ) ) ;
#23544 = ORIENTED_EDGE ( 'NONE', *, *, #18869, .F. ) ;
#23545 = CARTESIAN_POINT ( 'NONE',  ( 0.2819296736111110424, 0.2124999999241334314, 0.1167790944451424923 ) ) ;
#23546 = DIRECTION ( 'NONE',  ( 0.000000000000000000, 0.000000000000000000, -1.000000000000000000 ) ) ;
#23547 = DIRECTION ( 'NONE',  ( 0.08715574274765830465, -0.9961946980917454342, -3.870492493070289564E-17 ) ) ;
#23548 = PLANE ( 'NONE',  #16386 ) ;
#23549 = VECTOR ( 'NONE', #15170, 39.37007874015748143 ) ;
#23550 = CARTESIAN_POINT ( 'NONE',  ( -0.4000000000000000222, 0.08214285714285710083, 0.1299678784931624920 ) ) ;
#23551 = DIRECTION ( 'NONE',  ( 0.000000000000000000, 0.000000000000000000, -1.000000000000000000 ) ) ;
#23552 = DIRECTION ( 'NONE',  ( -0.4999999999999918954, 0.000000000000000000, -0.8660254037844432595 ) ) ;
#23553 = EDGE_CURVE ( 'NONE', #13418, #23454, #12078, .T. ) ;
#23554 = DIRECTION ( 'NONE',  ( -0.8320502943378444982, -0.4803844614152614767, -0.2773500981126123532 ) ) ;
#23555 = CARTESIAN_POINT ( 'NONE',  ( 5.178964085587577574E-17, 4.769527777853643791, 0.2819296736111110979 ) ) ;
#23556 = CARTESIAN_POINT ( 'NONE',  ( 0.08220319591558655770, 4.541475605104787761, -0.3014068057065943940 ) ) ;
#23557 = CARTESIAN_POINT ( 'NONE',  ( 0.1167790944451422702, 3.835500000075866556, -0.2819296736111110424 ) ) ;
#23558 = CARTESIAN_POINT ( 'NONE',  ( -0.1997126322592100711, 0.04726736168861581100, -0.2204034460251000083 ) ) ;
#23559 = CARTESIAN_POINT ( 'NONE',  ( 0.2841435314273037527, 5.033717116179627915, -0.1288771532856403945 ) ) ;
#23560 = LOCAL_TIME ( 21, 9, 13.00000000000000000, #3107 ) ;
#23561 = CARTESIAN_POINT ( 'NONE',  ( 0.1296959877176626363, 5.072999999999997733, 0.2866706542028402693 ) ) ;
#23562 = CARTESIAN_POINT ( 'NONE',  ( -0.008837736642443364682, 4.793618865691314568, 0.3119999992354540175 ) ) ;
#23563 = CC_DESIGN_PERSON_AND_ORGANIZATION_ASSIGNMENT ( #4688, #23327, ( #19252 ) ) ;
#23564 = CARTESIAN_POINT ( 'NONE',  ( -1.910449006669871087E-17, 4.321611111262843252, -0.3119999999999999996 ) ) ;
#23565 = CARTESIAN_POINT ( 'NONE',  ( 0.1167790944451422702, 4.793833333409199149, -0.2819296736111110979 ) ) ;
#23566 = ORIENTED_EDGE ( 'NONE', *, *, #9178, .F. ) ;
#23567 = CARTESIAN_POINT ( 'NONE',  ( -0.2819296736111110979, 3.741750000075865668, 0.000000000000000000 ) ) ;
#23568 = ORIENTED_EDGE ( 'NONE', *, *, #4689, .T. ) ;
#23569 = AXIS2_PLACEMENT_3D ( 'NONE', #17813, #23276, #6590 ) ;
#23570 = EDGE_LOOP ( 'NONE', ( #14407, #9322, #14021, #23880 ) ) ;
#23571 = PERSON_AND_ORGANIZATION ( #15518, #2538 ) ;
#23572 = CARTESIAN_POINT ( 'NONE',  ( 0.000000000000000000, 5.384999999999999787, -0.3119999999999999996 ) ) ;
#23573 = PLANE ( 'NONE',  #16297 ) ;
#23574 = LOCAL_TIME ( 21, 9, 13.00000000000000000, #9163 ) ;
#23575 = ORIENTED_EDGE ( 'NONE', *, *, #21241, .T. ) ;
#23576 = CARTESIAN_POINT ( 'NONE',  ( -0.2206173157302027954, 0.2541666665149337478, -0.2206173157302028232 ) ) ;
#23577 = CARTESIAN_POINT ( 'NONE',  ( -0.2378982579381299922, 4.384836116680865814, -0.2019271802617891021 ) ) ;
#23578 = CARTESIAN_POINT ( 'NONE',  ( -0.2742360776603882666, -0.1498359893665253684, -0.1016666666666679597 ) ) ;
#23579 = CARTESIAN_POINT ( 'NONE',  ( 0.1989806073349426052, 0.4406257711794490106, -0.7231433393460605652 ) ) ;
#23580 = ORIENTED_EDGE ( 'NONE', *, *, #3136, .F. ) ;
#23581 = DIRECTION ( 'NONE',  ( 0.000000000000000000, 0.000000000000000000, 1.000000000000000000 ) ) ;
#23582 = CARTESIAN_POINT ( 'NONE',  ( -0.1993543840281266633, 0.2229166665908000333, -0.1993543840281266910 ) ) ;
#23583 = CARTESIAN_POINT ( 'NONE',  ( -0.1954553509668046640, 0.1954553509668046918, 0.08138888888889070361 ) ) ;
#23584 = EDGE_CURVE ( 'NONE', #4696, #20991, #14714, .T. ) ;
#23585 = CARTESIAN_POINT ( 'NONE',  ( -0.2819296736111110424, 4.404944444520309865, -0.1167790944451423119 ) ) ;
#23586 = CARTESIAN_POINT ( 'NONE',  ( -0.03071979988719963223, 0.2873147545066508379, -0.07749523702218821808 ) ) ;
#23587 = CARTESIAN_POINT ( 'NONE',  ( -9.626299801968715084E-16, 0.4089285712334866374, -0.4000000000000000222 ) ) ;
#23588 = CARTESIAN_POINT ( 'NONE',  ( -0.01018560833394164394, 4.238034833529570555, 0.3119999986181690721 ) ) ;
#23589 = CARTESIAN_POINT ( 'NONE',  ( -0.1292346314604056745, 4.095916666666666650, -0.3119999999999999996 ) ) ;
#23590 = B_SPLINE_CURVE_WITH_KNOTS ( 'NONE', 3,
 ( #7414, #1679, #22281, #9112 ),
 .UNSPECIFIED., .F., .F.,
 ( 4, 4 ),
 ( 0.02432858112762273373, 0.08935694927272852528 ),
 .UNSPECIFIED. ) ;
#23591 = CARTESIAN_POINT ( 'NONE',  ( -1.910449006669871087E-17, 4.988277777929510215, -0.3119999999999999996 ) ) ;
#23592 = ADVANCED_FACE ( 'NONE', ( #14465 ), #1889, .F. ) ;
#23593 = CARTESIAN_POINT ( 'NONE',  ( -0.2923287055106771337, 0.2544642856167432798, -0.2123892367102620804 ) ) ;
#23594 = ORIENTED_EDGE ( 'NONE', *, *, #830, .T. ) ;
#23595 = DIRECTION ( 'NONE',  ( 0.000000000000000000, 0.000000000000000000, -1.000000000000000000 ) ) ;
#23596 = ORIENTED_EDGE ( 'NONE', *, *, #19160, .F. ) ;
#23597 = CARTESIAN_POINT ( 'NONE',  ( 0.000000000000000000, 2.735000000000000320, -0.4000000000000000222 ) ) ;
#23598 = VECTOR ( 'NONE', #14182, 39.37007874015748854 ) ;
#23599 = CARTESIAN_POINT ( 'NONE',  ( 0.3155070326520292290, 0.1306872919485615736, 0.3192361111111149397 ) ) ;
#23600 = CARTESIAN_POINT ( 'NONE',  ( -0.2233192592356399442, 0.3223214284738860624, -0.3073725909049500049 ) ) ;
#23601 = EDGE_LOOP ( 'NONE', ( #13022, #5022, #15434, #6011, #10010 ) ) ;
#23602 = CYLINDRICAL_SURFACE ( 'NONE', #18500, 0.3119999999999999996 ) ;
#23603 = EDGE_CURVE ( 'NONE', #14906, #4381, #9213, .T. ) ;
#23604 = EDGE_CURVE ( 'NONE', #17146, #16517, #3594, .T. ) ;
#23605 = CARTESIAN_POINT ( 'NONE',  ( 0.3613381517857143232, 0.1366071427596004251, 0.000000000000000000 ) ) ;
#23606 = EDGE_CURVE ( 'NONE', #8682, #5628, #9172, .T. ) ;
#23607 = CARTESIAN_POINT ( 'NONE',  ( -0.1993543840281266633, 0.1256944443685777957, -0.1993543840281266910 ) ) ;
#23608 = CARTESIAN_POINT ( 'NONE',  ( -0.1144950937579609779, 0.2764156081756484196, 0.08486111111111295513 ) ) ;
#23609 = CARTESIAN_POINT ( 'NONE',  ( -1.726321361862525858E-17, 5.241750000075865223, -0.2819296736111110979 ) ) ;
#23610 = CARTESIAN_POINT ( 'NONE',  ( -0.1954553509668046640, 0.1954553509668046918, 0.3661111111111151617 ) ) ;
#23611 = ORIENTED_EDGE ( 'NONE', *, *, #5846, .F. ) ;
#23612 = CARTESIAN_POINT ( 'NONE',  ( -0.01755531255181863592, 4.599896533210952931, -0.3115764429237145583 ) ) ;
#23613 = DIRECTION ( 'NONE',  ( 0.000000000000000000, 0.000000000000000000, 1.000000000000000000 ) ) ;
#23614 = CARTESIAN_POINT ( 'NONE',  ( 0.000000000000000000, 5.072999999999999510, 0.000000000000000000 ) ) ;
#23615 = CARTESIAN_POINT ( 'NONE',  ( 0.09694982473845883963, 0.06249891840240667101, 0.2965547697865978938 ) ) ;
#23616 = CARTESIAN_POINT ( 'NONE',  ( 0.3119999999999999996, 4.637583333333332725, -0.1292346314604056745 ) ) ;
#23617 = VECTOR ( 'NONE', #14640, 39.37007874015748143 ) ;
#23618 = CARTESIAN_POINT ( 'NONE',  ( 5.178964085587577574E-17, 4.033416666742532186, 0.2819296736111110979 ) ) ;
#23619 = CARTESIAN_POINT ( 'NONE',  ( 0.1167790944451422702, 3.849388888964754951, -0.2819296736111110424 ) ) ;
#23620 = EDGE_CURVE ( 'NONE', #1154, #10162, #5786, .T. ) ;
#23621 = LINE ( 'NONE', #3035, #4980 ) ;
#23622 = CARTESIAN_POINT ( 'NONE',  ( -0.008437752171424794251, 0.5369270166837832869, 0.04763592618482979241 ) ) ;
#23623 = ORIENTED_EDGE ( 'NONE', *, *, #20635, .T. ) ;
#23624 = CARTESIAN_POINT ( 'NONE',  ( -0.2819296736111110424, 4.578555555631421470, 0.1167790944451424923 ) ) ;
#23625 = CARTESIAN_POINT ( 'NONE',  ( -0.3062257137753721659, 4.500494688259138343, -0.05999501074661200278 ) ) ;
#23626 = PERSON_AND_ORGANIZATION_ROLE ( 'creator' ) ;
#23627 = CARTESIAN_POINT ( 'NONE',  ( -0.2195630361087207438, -0.1679215936615484350, -0.06558227484231504700 ) ) ;
#23628 = CARTESIAN_POINT ( 'NONE',  ( 0.1144950937579611444, 0.2764156081756483641, -0.04013888888888803713 ) ) ;
#23629 = VECTOR ( 'NONE', #14310, 39.37007874015748854 ) ;
#23630 = CARTESIAN_POINT ( 'NONE',  ( -0.1167790944451423535, 4.043833333409200037, 0.2819296736111110979 ) ) ;
#23631 = CARTESIAN_POINT ( 'NONE',  ( -0.2451711420345534798, 4.829615264078582548, -0.1970397708553964233 ) ) ;
#23632 = CARTESIAN_POINT ( 'NONE',  ( -0.3119999999999999996, 4.884111111111110404, 0.000000000000000000 ) ) ;
#23633 =( BOUNDED_CURVE ( )  B_SPLINE_CURVE ( 2, ( #1213, #21568, #12690, #20108, #10373, #17797, #3398, #15963, #16090 ),
 .UNSPECIFIED., .F., .T. ) 
 B_SPLINE_CURVE_WITH_KNOTS ( ( 3, 2, 2, 2, 3 ),
 ( 0.9375000000000001110, 0.9419642857142856984, 0.9464285714285712858, 0.9508928571428568732, 0.9553571428571425717 ),
 .UNSPECIFIED. ) 
 CURVE ( )  GEOMETRIC_REPRESENTATION_ITEM ( )  RATIONAL_B_SPLINE_CURVE ( ( 0.9999999999999981126, 0.9238795325112886259, 1.000000000000000000, 0.9238795325112867385, 1.000000000000000000, 0.9238795325112867385, 1.000000000000000000, 0.9238795325112924006, 0.9999999999999943379 ) ) 
 REPRESENTATION_ITEM ( '' )  );
#23634 = CARTESIAN_POINT ( 'NONE',  ( 0.000000000000000000, 3.700000000000000622, 0.000000000000000000 ) ) ;
#23635 = CARTESIAN_POINT ( 'NONE',  ( -6.979263641208234666E-17, -0.006250000097542401586, 0.3799334167787516425 ) ) ;
#23636 = CARTESIAN_POINT ( 'NONE',  ( 0.1993543840281266910, -0.01319444452031107509, -0.1993543840281266910 ) ) ;
#23637 = CARTESIAN_POINT ( 'NONE',  ( -0.2951834061891110417, 0.03795937687255804965, 0.4086815878027646454 ) ) ;
#23638 = DIRECTION ( 'NONE',  ( 0.000000000000000000, -0.9961946980917454342, 0.08715574274765833240 ) ) ;
#23639 = CARTESIAN_POINT ( 'NONE',  ( -0.1312060371020148941, 0.1993095342438279682, -0.7385277598563807500 ) ) ;
#23640 = CARTESIAN_POINT ( 'NONE',  ( -0.2230971623002954152, -0.2230971623002953874, 0.4581250000000046119 ) ) ;
#23641 = ORIENTED_EDGE ( 'NONE', *, *, #7113, .F. ) ;
#23642 = CARTESIAN_POINT ( 'NONE',  ( 0.2769159822048600783, 0.3938884537237697936, 0.07441357458167797978 ) ) ;
#23643 = CARTESIAN_POINT ( 'NONE',  ( 3.063257713472607067E-17, 5.580232050807569344, -0.2501339745962155581 ) ) ;
#23644 = CARTESIAN_POINT ( 'NONE',  ( -5.178964085587577574E-17, 0.4659722221463555858, 0.2819296736111110979 ) ) ;
#23645 = CARTESIAN_POINT ( 'NONE',  ( 0.2819296736111110424, 3.786888888964754507, -0.1167790944451423396 ) ) ;
#23646 = CARTESIAN_POINT ( 'NONE',  ( -0.1116596296178200276, 0.06160714275960046254, 0.3436530038418508792 ) ) ;
#23647 = EDGE_CURVE ( 'NONE', #45, #4381, #15408, .T. ) ;
#23648 = CARTESIAN_POINT ( 'NONE',  ( 0.1167790944451422702, 4.404944444520309865, -0.2819296736111110424 ) ) ;
#23649 = ADVANCED_FACE ( 'NONE', ( #13362 ), #13250, .T. ) ;
#23650 = CARTESIAN_POINT ( 'NONE',  ( -0.7171867353193159822, 1.999640111863030256, -2.958139940446594007 ) ) ;
#23651 = ORIENTED_EDGE ( 'NONE', *, *, #19200, .T. ) ;
#23652 = VECTOR ( 'NONE', #1713, 39.37007874015748854 ) ;
#23653 = LINE ( 'NONE', #12123, #760 ) ;
#23654 = CARTESIAN_POINT ( 'NONE',  ( -0.2819296736111110424, 5.189666666742532186, 0.1167790944451424923 ) ) ;
#23655 = CARTESIAN_POINT ( 'NONE',  ( 0.1831843189501979052, 4.204970245508889093, -0.2534774667974905027 ) ) ;
#23656 =( NAMED_UNIT ( * ) SI_UNIT ( $, .STERADIAN. ) SOLID_ANGLE_UNIT ( ) );
#23657 = LINE ( 'NONE', #5253, #1786 ) ;
#23658 = CARTESIAN_POINT ( 'NONE',  ( -0.2819296736111110979, 4.960500000075865223, -0.1167790944451422980 ) ) ;
#23659 = VERTEX_POINT ( 'NONE', #7854 ) ;
#23660 = DIRECTION ( 'NONE',  ( -1.000000000000000000, 0.000000000000000000, 0.000000000000000000 ) ) ;
#23661 = CARTESIAN_POINT ( 'NONE',  ( -0.07966684101420479225, 4.546095312717049808, -0.3042768302726782670 ) ) ;
#23662 = EDGE_LOOP ( 'NONE', ( #9320, #22874, #5159, #7042 ) ) ;
#23663 = CARTESIAN_POINT ( 'NONE',  ( -0.1993543840281267465, 0.3062499999241333759, 0.1993543840281266633 ) ) ;
#23664 = AXIS2_PLACEMENT_3D ( 'NONE', #9712, #17149, #439 ) ;
#23665 = ORIENTED_EDGE ( 'NONE', *, *, #3068, .F. ) ;
#23666 = DIRECTION ( 'NONE',  ( -0.000000000000000000, -1.000000000000000000, -0.000000000000000000 ) ) ;
#23667 = CARTESIAN_POINT ( 'NONE',  ( -0.3125913837188149524, 4.724895613529112026, 0.01951433487545338810 ) ) ;
#23668 = CARTESIAN_POINT ( 'NONE',  ( 0.3125000000000000000, -5.740531871003217465E-17, 0.2619444444444478659 ) ) ;
#23669 = CARTESIAN_POINT ( 'NONE',  ( -0.2472135954999579999, 0.08928571428571425994, 0.3402603233408159622 ) ) ;
#23670 = CARTESIAN_POINT ( 'NONE',  ( -0.3040973647138868752, 5.055585790322281170, -0.07619071978167928083 ) ) ;
#23671 = CARTESIAN_POINT ( 'NONE',  ( 3.820898013339742174E-17, 5.384999999999999787, 0.3119999999999999996 ) ) ;
#23672 = CARTESIAN_POINT ( 'NONE',  ( -0.2986281097515258720, 3.893695228114878226, 0.09285130349114770199 ) ) ;
#23673 = FACE_OUTER_BOUND ( 'NONE', #66, .T. ) ;
#23674 = CARTESIAN_POINT ( 'NONE',  ( -0.1993543840281266355, 4.429250000075866112, 0.1993543840281267465 ) ) ;
#23675 = CARTESIAN_POINT ( 'NONE',  ( 0.06631022961668026072, 4.541938770673441539, -0.3053197120535988129 ) ) ;
#23676 = CARTESIAN_POINT ( 'NONE',  ( -0.1167790944451423535, 5.154944444520309865, 0.2819296736111110424 ) ) ;
#23677 = FACE_OUTER_BOUND ( 'NONE', #1399, .T. ) ;
#23678 = CARTESIAN_POINT ( 'NONE',  ( 0.01543252246473785644, 3.738736189315518210, 0.3120000007626770877 ) ) ;
#23679 = DIRECTION ( 'NONE',  ( -0.000000000000000000, -1.000000000000000000, -0.000000000000000000 ) ) ;
#23680 = CARTESIAN_POINT ( 'NONE',  ( -0.1868639192671821270, 3.514980167629567998, 3.137089416182696322 ) ) ;
#23681 = B_SPLINE_CURVE_WITH_KNOTS ( 'NONE', 3,
 ( #13742, #10085, #22754, #7995, #4097, #22640 ),
 .UNSPECIFIED., .F., .F.,
 ( 4, 2, 4 ),
 ( 0.000000000000000000, 0.001246561431700771031, 0.002493122863401542495 ),
 .UNSPECIFIED. ) ;
#23682 = CARTESIAN_POINT ( 'NONE',  ( -0.1292346314604057023, 4.345916666818399499, 0.3119999999999998885 ) ) ;
#23683 = CARTESIAN_POINT ( 'NONE',  ( -0.2819296736111110979, 4.807722222298088433, -0.1167790944451422980 ) ) ;
#23684 = CARTESIAN_POINT ( 'NONE',  ( 0.2819296736111110424, 3.773000000075866112, -0.1167790944451423396 ) ) ;
#23685 = VECTOR ( 'NONE', #19094, 39.37007874015748854 ) ;
#23686 = ORIENTED_EDGE ( 'NONE', *, *, #20666, .F. ) ;
#23687 = EDGE_CURVE ( 'NONE', #22114, #9682, #21636, .T. ) ;
#23688 = PERSON_AND_ORGANIZATION ( #15518, #2538 ) ;
#23689 = CARTESIAN_POINT ( 'NONE',  ( 0.07527472113052306735, -0.4862786960646409140, 0.4165495381634258809 ) ) ;
#23690 = CARTESIAN_POINT ( 'NONE',  ( -0.3125000000000000555, 1.913510623667739771E-17, 0.2341666666666698537 ) ) ;
#23691 = ORIENTED_EDGE ( 'NONE', *, *, #19956, .F. ) ;
#23692 = CARTESIAN_POINT ( 'NONE',  ( -0.3119999999999999996, 0.2576388887371560132, -0.1292346314604056745 ) ) ;
#23693 = DIRECTION ( 'NONE',  ( -0.6123724356957930270, -0.7071067811865475727, 0.3535533905932765064 ) ) ;
#23694 = CC_DESIGN_DATE_AND_TIME_ASSIGNMENT ( #2338, #5623, ( #11949 ) ) ;
#23695 = CARTESIAN_POINT ( 'NONE',  ( -0.2017922277526993935, 3.716746900542896359, -0.2379588540888969983 ) ) ;
#23696 = CYLINDRICAL_SURFACE ( 'NONE', #13866, 0.3119999999999999996 ) ;
#23697 = CARTESIAN_POINT ( 'NONE',  ( 0.02825726476318201827, 0.5908114551644965129, -0.7495932795766503398 ) ) ;
#23698 = VERTEX_POINT ( 'NONE', #5904 ) ;
#23699 = ORIENTED_EDGE ( 'NONE', *, *, #226, .T. ) ;
#23700 = ORIENTED_EDGE ( 'NONE', *, *, #4798, .F. ) ;
#23701 = CARTESIAN_POINT ( 'NONE',  ( 0.1222830683586546147, 5.096320389118245586, -0.2862511053145868622 ) ) ;
#23702 = CARTESIAN_POINT ( 'NONE',  ( 1.726321361862525858E-17, 0.2715277777019111660, -0.2819296736111110979 ) ) ;
#23703 = CARTESIAN_POINT ( 'NONE',  ( 0.1954553509668046640, -0.1954553509668047195, 0.2202777777777807366 ) ) ;
#23704 = ORIENTED_EDGE ( 'NONE', *, *, #12041, .T. ) ;
#23705 = CARTESIAN_POINT ( 'NONE',  ( -0.1993543840281266355, 4.470916666742532186, 0.1993543840281267465 ) ) ;
#23706 = CYLINDRICAL_SURFACE ( 'NONE', #20800, 0.3119999999999999996 ) ;
#23707 = CARTESIAN_POINT ( 'NONE',  ( 0.000000000000000000, 5.580000000000000959, 0.000000000000000000 ) ) ;
#23708 = CARTESIAN_POINT ( 'NONE',  ( -0.2206173157302028787, 0.3791666665149337478, 0.2206173157302027954 ) ) ;
#23709 = CARTESIAN_POINT ( 'NONE',  ( 0.2206173157302027954, 4.029944444444443441, -0.2206173157302028232 ) ) ;
#23710 = CARTESIAN_POINT ( 'NONE',  ( 0.3119999999999999996, 4.970916666818399499, 0.1292346314604056190 ) ) ;
#23711 = CARTESIAN_POINT ( 'NONE',  ( -0.2206173157302028232, 4.154944444444443441, -0.2206173157302028232 ) ) ;
#23712 = CARTESIAN_POINT ( 'NONE',  ( -0.3037986732609906926, 4.893462023975497566, 0.08195073769739492919 ) ) ;
#23713 = AXIS2_PLACEMENT_3D ( 'NONE', #16632, #3332, #23802 ) ;
#23714 = EDGE_CURVE ( 'NONE', #8250, #12518, #22850, .T. ) ;
#23715 = CARTESIAN_POINT ( 'NONE',  ( 0.3155070326520292845, -5.795770164686806123E-17, 0.3713194444444487541 ) ) ;
#23716 = CARTESIAN_POINT ( 'NONE',  ( -0.2233192592356399997, 0.3437499999024575814, 0.3073725909049499494 ) ) ;
#23717 = B_SPLINE_CURVE_WITH_KNOTS ( 'NONE', 3,
 ( #7714, #20760, #4534, #15871, #10280, #8306, #4411, #8666, #21121, #1240, #876, #8183, #19648, #4651, #15759, #21246, #23289, #14049, #3069, #16116, #12120, #2822, #8552, #10039, #4892, #14166, #19528, #17826 ),
 .UNSPECIFIED., .F., .F.,
 ( 4, 2, 2, 2, 2, 2, 2, 2, 2, 2, 2, 2, 2, 4 ),
 ( 0.000000000000000000, 0.001089208970704103616, 0.002178417941408206365, 0.004356835882816414464, 0.005446044853520517863, 0.006535253824224622130, 0.007624462794928726396, 0.008713671765632828928, 0.009802880736336934062, 0.01089208970704103920, 0.01198129867774514606, 0.01307050764844925120, 0.01524892558985746667, 0.01742734353126568214 ),
 .UNSPECIFIED. ) ;
#23718 = CARTESIAN_POINT ( 'NONE',  ( 0.2534589807566784980, -0.3949312665968779945, 0.4181462219997758578 ) ) ;
#23719 = ADVANCED_FACE ( 'NONE', ( #2259 ), #176, .T. ) ;
#23720 = PRODUCT_DEFINITION_SHAPE ( 'NONE', 'NONE',  #24129 ) ;
#23721 = CARTESIAN_POINT ( 'NONE',  ( -0.2233192592356399997, 0.1116071427596004306, 0.3073725909049499494 ) ) ;
#23722 = CARTESIAN_POINT ( 'NONE',  ( 0.2819296736111110979, 0.2194444443685778234, -0.1167790944451422980 ) ) ;
#23723 = CARTESIAN_POINT ( 'NONE',  ( -0.1954553509668046640, 0.1954553509668046918, 0.1438888888888912032 ) ) ;
#23724 = CARTESIAN_POINT ( 'NONE',  ( -0.1167790944451423535, 5.099388888964754507, 0.2819296736111110424 ) ) ;
#23725 = CARTESIAN_POINT ( 'NONE',  ( 0.05028335205149757348, 4.486876821019038175, -0.3079317466717229612 ) ) ;
#23726 = ORIENTED_EDGE ( 'NONE', *, *, #14552, .T. ) ;
#23727 = CARTESIAN_POINT ( 'NONE',  ( 0.3120000000000000551, 3.852861111111110404, 0.1292346314604056190 ) ) ;
#23728 = CARTESIAN_POINT ( 'NONE',  ( -0.4749999999999999778, 3.575000000000000622, -0.09499999999999995948 ) ) ;
#23729 = CARTESIAN_POINT ( 'NONE',  ( -0.3125000000000000000, 3.738758431839877614E-19, -0.1016666666666665164 ) ) ;
#23730 = CARTESIAN_POINT ( 'NONE',  ( 0.2206173157302027676, 0.5597222220704892726, 0.2206173157302028787 ) ) ;
#23731 = CARTESIAN_POINT ( 'NONE',  ( 0.2206173157302028787, 4.682722222222222008, 0.2206173157302027954 ) ) ;
#23732 = TOROIDAL_SURFACE ( 'NONE', #7790, 0.3385998376278290256, 0.01874999999999999931 ) ;
#23733 = CARTESIAN_POINT ( 'NONE',  ( -1.726321361862525858E-17, 4.061194444520309865, -0.2819296736111110979 ) ) ;
#23734 = CARTESIAN_POINT ( 'NONE',  ( -0.2819296736111110424, 3.870222222298087988, 0.1167790944451424923 ) ) ;
#23735 = CARTESIAN_POINT ( 'NONE',  ( -0.3236067977499789694, 0.2142857142857142461, -0.2351141009169893104 ) ) ;
#23736 = CARTESIAN_POINT ( 'NONE',  ( -0.003294150194310526466, 0.5383638965977114443, 0.05893128447555143895 ) ) ;
#23737 = ORIENTED_EDGE ( 'NONE', *, *, #23959, .T. ) ;
#23738 = CARTESIAN_POINT ( 'NONE',  ( 5.731347020009612645E-17, 4.564666666666665762, 0.3119999999999999996 ) ) ;
#23739 = CARTESIAN_POINT ( 'NONE',  ( -0.1993543840281266355, 4.470916666742532186, 0.1993543840281267465 ) ) ;
#23740 = CARTESIAN_POINT ( 'NONE',  ( -0.2715579528645996055, 4.506751968752040760, 0.1545152121325979455 ) ) ;
#23741 = EDGE_CURVE ( 'NONE', #2652, #10864, #20903, .T. ) ;
#23742 = ADVANCED_FACE ( 'NONE', ( #6019 ), #298, .F. ) ;
#23743 = DATE_AND_TIME ( #16091, #4476 ) ;
#23744 = CARTESIAN_POINT ( 'NONE',  ( -0.4687500000000003886, -0.2598076211353319009, 0.06112444011295369711 ) ) ;
#23745 = VECTOR ( 'NONE', #6962, 39.37007874015748854 ) ;
#23746 = CARTESIAN_POINT ( 'NONE',  ( -0.1144950937579609779, 0.2764156081756484196, 0.1890277777777805146 ) ) ;
#23747 = CARTESIAN_POINT ( 'NONE',  ( 0.1993543840281266633, 4.068138888964754507, -0.1993543840281266910 ) ) ;
#23748 = CARTESIAN_POINT ( 'NONE',  ( -0.01875000000000017278, 0.5520911949125799634, 0.06112444011295375956 ) ) ;
#23749 = EDGE_CURVE ( 'NONE', #18459, #10673, #15182, .T. ) ;
#23750 = CARTESIAN_POINT ( 'NONE',  ( 0.04962117880717522439, 5.160786044563907993, -0.2954202128566375540 ) ) ;
#23751 = CARTESIAN_POINT ( 'NONE',  ( -0.4593750000000004219, 0.2760455974562897596, 0.06112444011295372487 ) ) ;
#23752 = CARTESIAN_POINT ( 'NONE',  ( 0.3119999999999999996, 0.06666666651493373397, 0.000000000000000000 ) ) ;
#23753 = CARTESIAN_POINT ( 'NONE',  ( -0.2923287055106771337, 0.1116071427596004306, -0.2123892367102620804 ) ) ;
#23754 = CARTESIAN_POINT ( 'NONE',  ( -0.2819296736111110979, 0.3444444443685779067, 0.1167790944451422425 ) ) ;
#23755 = DIRECTION ( 'NONE',  ( -0.08715574274765833240, 0.9961946980917454342, 3.870492493070290181E-17 ) ) ;
#23756 = DIRECTION ( 'NONE',  ( -0.000000000000000000, -1.000000000000000000, -0.000000000000000000 ) ) ;
#23757 = CARTESIAN_POINT ( 'NONE',  ( -7.000945310522701902E-17, 0.1678571428571427882, 0.3999999999999999667 ) ) ;
#23758 = CARTESIAN_POINT ( 'NONE',  ( -0.03651601414465285855, -0.2739930093161157543, -0.06558227484231510251 ) ) ;
#23759 = CARTESIAN_POINT ( 'NONE',  ( 0.1954553509668046640, -0.1954553509668047195, 0.06055555555555720143 ) ) ;
#23760 = ORIENTED_EDGE ( 'NONE', *, *, #14186, .F. ) ;
#23761 = ORIENTED_EDGE ( 'NONE', *, *, #3310, .T. ) ;
#23762 = LINE ( 'NONE', #10866, #16123 ) ;
#23763 = CARTESIAN_POINT ( 'NONE',  ( 2.824051777240061223E-14, 3.849388889040854522, 0.3119999999999999996 ) ) ;
#23764 = CARTESIAN_POINT ( 'NONE',  ( -5.731347020009612645E-17, 0.1152777777777774515, 0.3119999999999999996 ) ) ;
#23765 = CARTESIAN_POINT ( 'NONE',  ( -0.2819296736111110424, 3.814666666742532630, 0.1167790944451424923 ) ) ;
#23766 = CARTESIAN_POINT ( 'NONE',  ( -0.3613381517857143232, 0.1151785713310290032, -0.1174058825155741004 ) ) ;
#23767 = CARTESIAN_POINT ( 'NONE',  ( 0.1167790944451424368, 4.328555555631420582, 0.2819296736111110424 ) ) ;
#23768 = LINE ( 'NONE', #11230, #19387 ) ;
#23769 = CARTESIAN_POINT ( 'NONE',  ( -0.3119999999999999996, 0.1499999998482670627, -3.820898013339742174E-17 ) ) ;
#23770 = CIRCLE ( 'NONE', #10577, 0.1850000000000000533 ) ;
#23771 = ORIENTED_EDGE ( 'NONE', *, *, #2023, .T. ) ;
#23772 = CARTESIAN_POINT ( 'NONE',  ( 0.1292346314604070623, 4.679249999999999687, 0.3119999999999986673 ) ) ;
#23773 = CARTESIAN_POINT ( 'NONE',  ( 0.1167790944451424368, 5.203555555631421470, 0.2819296736111110424 ) ) ;
#23774 = CARTESIAN_POINT ( 'NONE',  ( 0.3011295810430658082, 4.199072593115692698, -0.08461153459480627581 ) ) ;
#23775 =( BOUNDED_CURVE ( )  B_SPLINE_CURVE ( 2, ( #14531, #23890, #16715, #16239, #20012, #7209, #3423, #1478, #21723 ),
 .UNSPECIFIED., .F., .T. ) 
 B_SPLINE_CURVE_WITH_KNOTS ( ( 3, 2, 2, 2, 3 ),
 ( 0.5624999999999998890, 0.5669642857142855874, 0.5714285714285711748, 0.5758928571428568732, 0.5803571428571426827 ),
 .UNSPECIFIED. ) 
 CURVE ( )  GEOMETRIC_REPRESENTATION_ITEM ( )  RATIONAL_B_SPLINE_CURVE ( ( 1.000000000000001998, 0.9238795325112848511, 1.000000000000000000, 0.9238795325112867385, 1.000000000000000000, 0.9238795325112867385, 1.000000000000000000, 0.9238795325112905132, 0.9999999999999962252 ) ) 
 REPRESENTATION_ITEM ( '' )  );
#23776 = DIRECTION ( 'NONE',  ( 0.000000000000000000, 0.000000000000000000, 1.000000000000000000 ) ) ;
#23777 =( BOUNDED_CURVE ( )  B_SPLINE_CURVE ( 2, ( #8563, #10525, #1249, #12483, #19902, #3311, #12132, #3191, #10639 ),
 .UNSPECIFIED., .F., .T. ) 
 B_SPLINE_CURVE_WITH_KNOTS ( ( 3, 2, 2, 2, 3 ),
 ( 0.4375000000000000000, 0.4479166666666666852, 0.4583333333333333148, 0.4687500000000000000, 0.4791666666666666852 ),
 .UNSPECIFIED. ) 
 CURVE ( )  GEOMETRIC_REPRESENTATION_ITEM ( )  RATIONAL_B_SPLINE_CURVE ( ( 1.000000000000000000, 0.9238795325112867385, 1.000000000000000000, 0.9238795325112867385, 1.000000000000000000, 0.9238795325112867385, 1.000000000000000000, 0.9238795325112867385, 1.000000000000000000 ) ) 
 REPRESENTATION_ITEM ( '' )  );
#23778 = CARTESIAN_POINT ( 'NONE',  ( 0.2819296736111110979, 4.880638888964754507, -3.452642723725051716E-17 ) ) ;
#23779 = CONTEXT_DEPENDENT_SHAPE_REPRESENTATION ( #10926, #16357 ) ;
#23780 = EDGE_CURVE ( 'NONE', #314, #15906, #4522, .T. ) ;
#23781 = CARTESIAN_POINT ( 'NONE',  ( -0.1549220363945191525, 4.066990437257307356, 0.2708196028344186379 ) ) ;
#23782 = CARTESIAN_POINT ( 'NONE',  ( 0.3119999999999999996, 4.911888888888888083, -3.820898013339742174E-17 ) ) ;
#23783 = ORIENTED_EDGE ( 'NONE', *, *, #6893, .T. ) ;
#23784 = CARTESIAN_POINT ( 'NONE',  ( -0.1993543840281266633, 0.2923611110352444808, -0.1993543840281266910 ) ) ;
#23785 = VECTOR ( 'NONE', #20418, 39.37007874015748143 ) ;
#23786 = ORIENTED_EDGE ( 'NONE', *, *, #16243, .F. ) ;
#23787 = CARTESIAN_POINT ( 'NONE',  ( -0.1167790944451424368, 0.03194444436857781650, 0.2819296736111110424 ) ) ;
#23788 = FACE_OUTER_BOUND ( 'NONE', #4087, .T. ) ;
#23789 = LINE ( 'NONE', #12974, #12498 ) ;
#23790 = CARTESIAN_POINT ( 'NONE',  ( -0.3236067977499789694, -1.707404996040164512E-17, -0.2351141009169893104 ) ) ;
#23791 = CARTESIAN_POINT ( 'NONE',  ( 0.3155070326520292290, -0.1306872919485616569, -0.08006944444444412390 ) ) ;
#23792 = DIRECTION ( 'NONE',  ( 0.8651979924482660067, -0.04370253788966849823, -0.4995222938423193870 ) ) ;
#23793 = DIRECTION ( 'NONE',  ( -1.000000000000000000, -0.000000000000000000, -0.000000000000000000 ) ) ;
#23794 = CARTESIAN_POINT ( 'NONE',  ( 0.9657290084419611897, 2.439517176785165997, -1.274898457470592605 ) ) ;
#23795 = CARTESIAN_POINT ( 'NONE',  ( -0.1993543840281266355, 4.595916666742532186, 0.1993543840281267465 ) ) ;
#23796 = FACE_BOUND ( 'NONE', #21321, .T. ) ;
#23797 = CARTESIAN_POINT ( 'NONE',  ( -5.731347020009612645E-17, 0.2749999998482670627, 0.3119999999999999996 ) ) ;
#23798 = CARTESIAN_POINT ( 'NONE',  ( 0.1167790944451424368, 4.995222222298087544, 0.2819296736111110424 ) ) ;
#23799 = LINE ( 'NONE', #7120, #15775 ) ;
#23800 = CARTESIAN_POINT ( 'NONE',  ( 0.2911863994614913853, 3.755533081060165923, -0.1151799365104299866 ) ) ;
#23801 = DIRECTION ( 'NONE',  ( 0.000000000000000000, 0.000000000000000000, -1.000000000000000000 ) ) ;
#23802 = DIRECTION ( 'NONE',  ( -1.000000000000000000, 0.000000000000000000, 0.000000000000000000 ) ) ;
#23803 = CARTESIAN_POINT ( 'NONE',  ( -0.1292346314604056745, 4.269527777929510215, -0.3119999999999999996 ) ) ;
#23804 = CARTESIAN_POINT ( 'NONE',  ( -0.2819296736111110979, 4.585500000075865223, -0.1167790944451422980 ) ) ;
#23805 = CARTESIAN_POINT ( 'NONE',  ( -0.1167790944451423257, 3.786888888964754063, -0.2819296736111110424 ) ) ;
#23806 = VERTEX_POINT ( 'NONE', #6140 ) ;
#23807 = VERTEX_POINT ( 'NONE', #2382 ) ;
#23808 = ORIENTED_EDGE ( 'NONE', *, *, #18104, .F. ) ;
#23809 = APPROVAL_DATE_TIME ( #10797, #15656 ) ;
#23810 = CARTESIAN_POINT ( 'NONE',  ( 0.4607728391470888862, -0.2757711312522246327, 0.04763613967037444441 ) ) ;
#23811 = EDGE_CURVE ( 'NONE', #2014, #17381, #9451, .T. ) ;
#23812 = CARTESIAN_POINT ( 'NONE',  ( -0.08150439437264625497, 4.958142549569055646, 0.3039118706599210351 ) ) ;
#23813 = DIRECTION ( 'NONE',  ( 1.000000000000000000, 0.000000000000000000, 0.000000000000000000 ) ) ;
#23814 = EDGE_LOOP ( 'NONE', ( #11820, #5048 ) ) ;
#23815 = CARTESIAN_POINT ( 'NONE',  ( -0.3119999999999999996, 0.2645833331816004330, 0.1292346314604056190 ) ) ;
#23816 = CARTESIAN_POINT ( 'NONE',  ( -0.2346756888474252623, 4.397428374997647715, 0.2066071494487769222 ) ) ;
#23817 = CARTESIAN_POINT ( 'NONE',  ( -0.2009661027989112503, 3.716715306565030019, -0.2386561446537507347 ) ) ;
#23818 = CARTESIAN_POINT ( 'NONE',  ( -5.731347020009612645E-17, 0.2819444444444441089, 0.3119999999999999996 ) ) ;
#23819 = CARTESIAN_POINT ( 'NONE',  ( 0.2105398893019958806, 0.3855051204502836781, -0.7198424012877072675 ) ) ;
#23820 = VERTEX_POINT ( 'NONE', #9818 ) ;
#23821 = ORIENTED_EDGE ( 'NONE', *, *, #8425, .F. ) ;
#23822 = APPLICATION_CONTEXT ( 'configuration controlled 3d designs of mechanical parts and assemblies' ) ;
#23823 = ORIENTED_EDGE ( 'NONE', *, *, #9458, .F. ) ;
#23824 = CARTESIAN_POINT ( 'NONE',  ( 0.06994230879797320999, 5.073571722091643643, 0.3046847899301766138 ) ) ;
#23825 = CARTESIAN_POINT ( 'NONE',  ( 0.1954553509668047195, 0.1954553509668046085, 0.2341666666666697150 ) ) ;
#23826 = CARTESIAN_POINT ( 'NONE',  ( -0.1993543840281266910, 4.123694444520309865, -0.1993543840281266910 ) ) ;
#23827 = CARTESIAN_POINT ( 'NONE',  ( -0.1993543840281266910, 5.012583333409199149, -0.1993543840281266910 ) ) ;
#23828 = CARTESIAN_POINT ( 'NONE',  ( -0.08208976641702336874, -0.4938713286266925850, 0.4000323696459241463 ) ) ;
#23829 = CARTESIAN_POINT ( 'NONE',  ( -0.3085935790486541430, 4.225662198787177637, 0.04598119064307899101 ) ) ;
#23830 = CARTESIAN_POINT ( 'NONE',  ( -0.2206173157302027676, 4.168833333333332725, 0.2206173157302028787 ) ) ;
#23831 = CARTESIAN_POINT ( 'NONE',  ( -0.1292346314604056745, 5.047305555707287894, -0.3119999999999999996 ) ) ;
#23832 = VECTOR ( 'NONE', #9974, 39.37007874015748143 ) ;
#23833 = CARTESIAN_POINT ( 'NONE',  ( -0.1993543840281266910, 5.082027777853643791, -0.1993543840281266910 ) ) ;
#23834 = CARTESIAN_POINT ( 'NONE',  ( -1.910449006669871087E-17, 4.147999999999998799, -0.3119999999999999996 ) ) ;
#23835 = ORIENTED_EDGE ( 'NONE', *, *, #1891, .T. ) ;
#23836 = CARTESIAN_POINT ( 'NONE',  ( -0.07783884650168826358, 0.05932970560135347043, 0.2990238257868908511 ) ) ;
#23837 = VERTEX_POINT ( 'NONE', #20782 ) ;
#23838 = CARTESIAN_POINT ( 'NONE',  ( 0.2230971623002953874, -0.2230971623002954429, 0.1977083333333363169 ) ) ;
#23839 = CARTESIAN_POINT ( 'NONE',  ( -0.3613381517857143232, 0.4044642856167432465, -4.425116109941954795E-17 ) ) ;
#23840 = ORIENTED_EDGE ( 'NONE', *, *, #2280, .T. ) ;
#23841 = VECTOR ( 'NONE', #12591, 39.37007874015748143 ) ;
#23842 = CARTESIAN_POINT ( 'NONE',  ( 0.1236067977499789861, 0.05714285714285712720, -0.3804226065180614236 ) ) ;
#23843 = CARTESIAN_POINT ( 'NONE',  ( 0.2233192592356399997, 0.3616071427596004861, -0.3073725909049500049 ) ) ;
#23844 = CARTESIAN_POINT ( 'NONE',  ( -5.178964085587577574E-17, 0.2576388888130222155, 0.2819296736111110979 ) ) ;
#23845 = CARTESIAN_POINT ( 'NONE',  ( 0.2764156081756484196, -5.077672346800151106E-17, 0.1786111111111136907 ) ) ;
#23846 = CARTESIAN_POINT ( 'NONE',  ( 0.1993543840281266633, 5.123694444520309865, -0.1993543840281266910 ) ) ;
#23847 = CARTESIAN_POINT ( 'NONE',  ( 0.05305093651153936635, 4.486802096876033374, -0.3074566729606528215 ) ) ;
#23848 = ORIENTED_EDGE ( 'NONE', *, *, #11755, .T. ) ;
#23849 = CARTESIAN_POINT ( 'NONE',  ( -1.726321361862525858E-17, 4.783416666742532186, -0.2819296736111110979 ) ) ;
#23850 = PLANE ( 'NONE',  #2881 ) ;
#23851 = EDGE_CURVE ( 'NONE', #23209, #19709, #4902, .T. ) ;
#23852 = LINE ( 'NONE', #20457, #4686 ) ;
#23853 = CARTESIAN_POINT ( 'NONE',  ( 0.2206173157302028787, 4.071611111111110404, 0.2206173157302027954 ) ) ;
#23854 = CARTESIAN_POINT ( 'NONE',  ( -0.4723904922468886158, 0.2801879233228458665, 0.04193467568257214922 ) ) ;
#23855 = CARTESIAN_POINT ( 'NONE',  ( -0.3119999999999998885, 4.665361111111110404, 0.1292346314604058410 ) ) ;
#23856 = CARTESIAN_POINT ( 'NONE',  ( -0.1167790944451423119, 4.009111111186976828, -0.2819296736111110979 ) ) ;
#23857 = CARTESIAN_POINT ( 'NONE',  ( -0.2819296736111110979, 3.866750000075866112, 0.000000000000000000 ) ) ;
#23858 = CARTESIAN_POINT ( 'NONE',  ( 0.2904387420176882117, 4.033251672939094590, -0.1141962754506169742 ) ) ;
#23859 = LINE ( 'NONE', #18153, #3543 ) ;
#23860 = ORIENTED_EDGE ( 'NONE', *, *, #18001, .T. ) ;
#23861 = CARTESIAN_POINT ( 'NONE',  ( -1.910449006669871087E-17, 3.925777777777776922, -0.3119999999999999996 ) ) ;
#23862 = ORIENTED_EDGE ( 'NONE', *, *, #15431, .F. ) ;
#23863 = CARTESIAN_POINT ( 'NONE',  ( -0.1993543840281266355, 4.359805555631421470, 0.1993543840281267465 ) ) ;
#23864 = CIRCLE ( 'NONE', #4433, 0.01874999999999997155 ) ;
#23865 = EDGE_CURVE ( 'NONE', #23140, #4857, #10767, .T. ) ;
#23866 = CARTESIAN_POINT ( 'NONE',  ( -0.2830962153688056371, 4.498198518508631949, -0.1381818899629860820 ) ) ;
#23867 = CARTESIAN_POINT ( 'NONE',  ( -0.1060554323913378977, 1.041821957232212270, -2.874935959385435336 ) ) ;
#23868 = CARTESIAN_POINT ( 'NONE',  ( 0.000000000000000000, 0.2764156081756484196, 0.2966666666666702423 ) ) ;
#23869 = CARTESIAN_POINT ( 'NONE',  ( -0.1571291514452808069, 3.955868408054724394, 0.2726213375442139708 ) ) ;
#23870 = CARTESIAN_POINT ( 'NONE',  ( -0.1571085868019625187, 4.455918294536927782, 0.2726333643457281020 ) ) ;
#23871 = CARTESIAN_POINT ( 'NONE',  ( 0.1292346314604056745, 0.07708333318160039138, -0.3119999999999999996 ) ) ;
#23872 = CARTESIAN_POINT ( 'NONE',  ( 2.326421213736078119E-17, 0.3151785713310290005, -0.3799334167787516425 ) ) ;
#23873 = CARTESIAN_POINT ( 'NONE',  ( -0.2819296736111110424, 0.1708333332574666907, -0.1167790944451423396 ) ) ;
#23874 = CARTESIAN_POINT ( 'NONE',  ( 0.0001582775150950677980, 3.877162414149467828, -0.3119999700502704143 ) ) ;
#23875 = CARTESIAN_POINT ( 'NONE',  ( 0.3119999999999999996, 0.5770833333333330595, -0.1292346314604056468 ) ) ;
#23876 = CARTESIAN_POINT ( 'NONE',  ( 0.4449999999999991740, 2.740000000000000213, 0.000000000000000000 ) ) ;
#23877 = CARTESIAN_POINT ( 'NONE',  ( -0.1954553509668046918, -0.1954553509668046640, 0.04666666666666818841 ) ) ;
#23878 = AXIS2_PLACEMENT_3D ( 'NONE', #4402, #6230, #17454 ) ;
#23879 = ORIENTED_EDGE ( 'NONE', *, *, #12017, .T. ) ;
#23880 = ORIENTED_EDGE ( 'NONE', *, *, #9432, .F. ) ;
#23881 = CARTESIAN_POINT ( 'NONE',  ( 6.388359114324787822E-07, 4.627192232271967853, 0.3119999999985919592 ) ) ;
#23882 = CARTESIAN_POINT ( 'NONE',  ( -0.3125000000000000000, 0.000000000000000000, 1.326383476483184332 ) ) ;
#23883 = CARTESIAN_POINT ( 'NONE',  ( -0.3119999999999999996, -0.01319444444444478094, -0.1292346314604056745 ) ) ;
#23884 = EDGE_CURVE ( 'NONE', #13239, #2823, #15069, .T. ) ;
#23885 = CARTESIAN_POINT ( 'NONE',  ( 5.178964085587577574E-17, 3.825083333409199149, 0.2819296736111110979 ) ) ;
#23886 = CARTESIAN_POINT ( 'NONE',  ( 0.3613381517857143232, 0.2294642856167433131, -0.1174058825155740587 ) ) ;
#23887 = ORIENTED_EDGE ( 'NONE', *, *, #3485, .F. ) ;
#23888 = CARTESIAN_POINT ( 'NONE',  ( -0.1167790944451423535, 4.432722222298088433, 0.2819296736111110424 ) ) ;
#23889 = DIRECTION ( 'NONE',  ( -0.4985709748471496283, -0.07555085810113111588, -0.8635502596144277732 ) ) ;
#23890 = CARTESIAN_POINT ( 'NONE',  ( -0.1292346314604032875, 4.394527777777778255, 0.3120000000000023865 ) ) ;
#23891 = EDGE_LOOP ( 'NONE', ( #20640, #1793, #23141, #6960 ) ) ;
#23892 = CARTESIAN_POINT ( 'NONE',  ( 1.364852645245658621E-07, 4.377166663151471404, -0.3119999999999701346 ) ) ;
#23893 = CARTESIAN_POINT ( 'NONE',  ( -0.1167790944451423535, 5.141055555631421470, 0.2819296736111110424 ) ) ;
#23894 = EDGE_CURVE ( 'NONE', #11233, #4444, #5130, .T. ) ;
#23895 = CARTESIAN_POINT ( 'NONE',  ( 0.2345140992797901391, 4.203002459309779226, -0.2057879445052058498 ) ) ;
#23896 = VECTOR ( 'NONE', #1440, 39.37007874015748143 ) ;
#23897 = CARTESIAN_POINT ( 'NONE',  ( 0.7463359724041155330, 0.2080000000000005456, -2.749000000000000554 ) ) ;
#23898 = DIRECTION ( 'NONE',  ( 0.000000000000000000, 1.000000000000000000, 0.000000000000000000 ) ) ;
#23899 = CARTESIAN_POINT ( 'NONE',  ( -0.1993543840281266910, 4.734805555631420582, -0.1993543840281266910 ) ) ;
#23900 = CALENDAR_DATE ( 2026, 7, 10 ) ;
#23901 = CARTESIAN_POINT ( 'NONE',  ( 5.574357792518489764E-07, 4.071633398088104094, 0.3119999999989289674 ) ) ;
#23902 = EDGE_CURVE ( 'NONE', #14094, #8085, #13820, .T. ) ;
#23903 = CARTESIAN_POINT ( 'NONE',  ( 0.1292346314604027324, 4.901472222222221120, 0.3120000000000029972 ) ) ;
#23904 = VECTOR ( 'NONE', #23898, 39.37007874015748143 ) ;
#23905 = CARTESIAN_POINT ( 'NONE',  ( 0.1167790944451423257, 0.2263888888130222710, -0.2819296736111110424 ) ) ;
#23906 = ORIENTED_EDGE ( 'NONE', *, *, #22448, .F. ) ;
#23907 = CARTESIAN_POINT ( 'NONE',  ( -5.178964085587577574E-17, 0.1465277777019111383, 0.2819296736111110979 ) ) ;
#23908 = CARTESIAN_POINT ( 'NONE',  ( 5.731347020009612645E-17, 4.342444444444443441, 0.3119999999999999996 ) ) ;
#23909 = CARTESIAN_POINT ( 'NONE',  ( -0.2705232885797667075, 5.199178293702563458, -0.09182951230709678059 ) ) ;
#23910 = CARTESIAN_POINT ( 'NONE',  ( 0.3999999999999999667, 0.03928571428571425023, 0.1299678784931626307 ) ) ;
#23911 = CARTESIAN_POINT ( 'NONE',  ( -0.3155070326520292845, 1.931923388228935888E-17, -0.04881944444444386716 ) ) ;
#23912 = LINE ( 'NONE', #18081, #12241 ) ;
#23913 = CARTESIAN_POINT ( 'NONE',  ( -0.3073899478517820305, 3.889436215408048625, -0.05583288564120540698 ) ) ;
#23914 = CARTESIAN_POINT ( 'NONE',  ( 1.726321361862525858E-17, 0.1048611110352444808, -0.2819296736111110979 ) ) ;
#23915 = EDGE_CURVE ( 'NONE', #7560, #21247, #14327, .T. ) ;
#23916 = ADVANCED_FACE ( 'NONE', ( #20380 ), #21961, .T. ) ;
#23917 = CARTESIAN_POINT ( 'NONE',  ( -0.1167790944451423535, 4.543833333409199149, 0.2819296736111110424 ) ) ;
#23918 = CARTESIAN_POINT ( 'NONE',  ( 0.3236067977499789694, 0.09821428551920091676, 0.2351141009169893659 ) ) ;
#23919 = CARTESIAN_POINT ( 'NONE',  ( 7.284403261834130553E-05, 4.543831265541522946, -0.3120000004383560732 ) ) ;
#23920 = AXIS2_PLACEMENT_3D ( 'NONE', #11547, #438, #20683 ) ;
#23921 = CARTESIAN_POINT ( 'NONE',  ( 0.2819296736111110424, 5.120222222298088433, -0.1167790944451423396 ) ) ;
#23922 = CARTESIAN_POINT ( 'NONE',  ( 0.4593750000000002554, -1.978974282089605735E-13, 0.4343810118395207698 ) ) ;
#23923 = CARTESIAN_POINT ( 'NONE',  ( 0.1916526620523836544, 4.910811664053455594, 0.2495586235085527904 ) ) ;
#23924 = DIRECTION ( 'NONE',  ( -0.000000000000000000, -1.000000000000000000, -0.000000000000000000 ) ) ;
#23925 = CARTESIAN_POINT ( 'NONE',  ( -0.1583113556673881317, 0.4498647735549333726, 0.08855526556985508779 ) ) ;
#23926 = CARTESIAN_POINT ( 'NONE',  ( -0.3119999999999999996, 4.224388889040620931, 0.000000000000000000 ) ) ;
#23927 = EDGE_CURVE ( 'NONE', #11483, #21966, #24025, .T. ) ;
#23928 = CARTESIAN_POINT ( 'NONE',  ( 0.2819296736111110979, 4.505638888964754507, -3.452642723725051716E-17 ) ) ;
#23929 =( BOUNDED_CURVE ( )  B_SPLINE_CURVE ( 2, ( #13164, #23984, #3755, #22040, #7652, #5816, #23853, #7172, #5335 ),
 .UNSPECIFIED., .F., .T. ) 
 B_SPLINE_CURVE_WITH_KNOTS ( ( 3, 2, 2, 2, 3 ),
 ( 0.7589285714285712858, 0.7633928571428570953, 0.7678571428571430157, 0.7723214285714287142, 0.7767857142857145236 ),
 .UNSPECIFIED. ) 
 CURVE ( )  GEOMETRIC_REPRESENTATION_ITEM ( )  RATIONAL_B_SPLINE_CURVE ( ( 1.000000000000001998, 0.9238795325112848511, 1.000000000000000000, 0.9238795325112867385, 1.000000000000000000, 0.9238795325112867385, 1.000000000000000000, 0.9238795325112829637, 1.000000000000003775 ) ) 
 REPRESENTATION_ITEM ( '' )  );
#23930 =( BOUNDED_CURVE ( )  B_SPLINE_CURVE ( 2, ( #849, #6453, #2793, #23499, #14135, #4736, #12441, #13906, #15843 ),
 .UNSPECIFIED., .F., .F. ) 
 B_SPLINE_CURVE_WITH_KNOTS ( ( 3, 2, 2, 2, 3 ),
 ( 0.4895833333333334814, 0.5000000000000001110, 0.5104166666666668517, 0.5208333333333334814, 0.5312500000000001110 ),
 .UNSPECIFIED. ) 
 CURVE ( )  GEOMETRIC_REPRESENTATION_ITEM ( )  RATIONAL_B_SPLINE_CURVE ( ( 0.9999999999999992228, 0.9238795325112875156, 1.000000000000000000, 0.9238795325112867385, 1.000000000000000000, 0.9238795325112867385, 1.000000000000000000, 0.9238795325112859613, 1.000000000000000888 ) ) 
 REPRESENTATION_ITEM ( '' )  );
#23931 = CC_DESIGN_APPROVAL ( #15224, ( #5255 ) ) ;
#23932 = CARTESIAN_POINT ( 'NONE',  ( 0.2819296736111110979, 3.880638888964754063, -3.452642723725051716E-17 ) ) ;
#23933 = PRODUCT_DEFINITION_SHAPE ( 'NONE', 'NONE',  #24131 ) ;
#23934 = ORIENTED_EDGE ( 'NONE', *, *, #7098, .T. ) ;
#23935 = EDGE_LOOP ( 'NONE', ( #18906, #12006, #6911, #7131 ) ) ;
#23936 = CALENDAR_DATE ( 2026, 7, 10 ) ;
#23937 = CARTESIAN_POINT ( 'NONE',  ( 0.01239990016126697736, -0.3069330571738623781, 0.4183927809049745594 ) ) ;
#23938 = VECTOR ( 'NONE', #14356, 39.37007874015748143 ) ;
#23939 = CARTESIAN_POINT ( 'NONE',  ( -0.3119332791068817889, 4.947851738477909045, 0.04138887372432151907 ) ) ;
#23940 = CARTESIAN_POINT ( 'NONE',  ( -0.5116234456863258950, 5.071846480923144718, -2.831306746567448407 ) ) ;
#23941 = EDGE_LOOP ( 'NONE', ( #22239, #13376, #10067, #12295 ) ) ;
#23942 = CARTESIAN_POINT ( 'NONE',  ( -0.1292346314604058410, 0.3270833331816004330, 0.3119999999999998885 ) ) ;
#23943 = CARTESIAN_POINT ( 'NONE',  ( -0.1294417382415922746, -0.3125000000000000000, 0.1890277777777807366 ) ) ;
#23944 = CARTESIAN_POINT ( 'NONE',  ( -0.3148642296646037009, 3.724867759073636542, 0.01804088196266112956 ) ) ;
#23945 = CARTESIAN_POINT ( 'NONE',  ( -0.5116234456863258950, 1.999640111863029812, -2.817014339916372290 ) ) ;
#23946 = CARTESIAN_POINT ( 'NONE',  ( 0.8977114317029943891, 0.000000000000000000, -0.4292782587447178111 ) ) ;
#23947 = ORIENTED_EDGE ( 'NONE', *, *, #17389, .T. ) ;
#23948 = ORIENTED_EDGE ( 'NONE', *, *, #13525, .F. ) ;
#23949 = CC_DESIGN_SECURITY_CLASSIFICATION ( #5255, ( #7598 ) ) ;
#23950 = CARTESIAN_POINT ( 'NONE',  ( -0.2923287055106771337, 0.1973214284738861179, 0.2123892367102619971 ) ) ;
#23951 = ORIENTED_EDGE ( 'NONE', *, *, #9831, .F. ) ;
#23952 = CARTESIAN_POINT ( 'NONE',  ( 0.1756681423353473881, 5.076946340042797878, 0.2579994535246159515 ) ) ;
#23953 = CARTESIAN_POINT ( 'NONE',  ( 0.1144950937579611444, 0.2764156081756483641, 0.2376388888888919526 ) ) ;
#23954 = CARTESIAN_POINT ( 'NONE',  ( -0.1167790944451423535, 4.307722222298088433, 0.2819296736111110424 ) ) ;
#23955 = CARTESIAN_POINT ( 'NONE',  ( -0.2819296736111110424, 5.189666666742532186, 0.1167790944451424923 ) ) ;
#23956 = CARTESIAN_POINT ( 'NONE',  ( 0.1537937564251784239, -0.2409193255903653574, 0.3973559490783071801 ) ) ;
#23957 = CARTESIAN_POINT ( 'NONE',  ( 6.089848770316828444E-07, 4.238302053322364316, 0.3119999999987258521 ) ) ;
#23958 = CARTESIAN_POINT ( 'NONE',  ( 0.3119999999999999996, 3.859805555555555046, -0.1292346314604056745 ) ) ;
#23959 = EDGE_CURVE ( 'NONE', #14094, #4761, #14201, .T. ) ;
#23960 = CARTESIAN_POINT ( 'NONE',  ( -1.910449006669871087E-17, 5.043833333485064685, -0.3119999999999999996 ) ) ;
#23961 = VECTOR ( 'NONE', #7022, 39.37007874015748143 ) ;
#23962 = ADVANCED_FACE ( 'NONE', ( #14662 ), #11240, .T. ) ;
#23963 = CARTESIAN_POINT ( 'NONE',  ( 0.1993543840281267465, 5.165361111186976828, 0.1993543840281266633 ) ) ;
#23964 = DIRECTION ( 'NONE',  ( -1.000000000000000000, 0.000000000000000000, 0.000000000000000000 ) ) ;
#23965 = VERTEX_POINT ( 'NONE', #1722 ) ;
#23966 = CC_DESIGN_APPROVAL ( #5523, ( #4115 ) ) ;
#23967 = PERSON ( 'NAUO-PER3', 'UNSPECIFIED', 'UNSPECIFIED', ('UNSPECIFIED'), ('UNSPECIFIED'), ('UNSPECIFIED') ) ;
#23968 = DIRECTION ( 'NONE',  ( -1.000000000000000000, 0.000000000000000000, 0.000000000000000000 ) ) ;
#23969 = CARTESIAN_POINT ( 'NONE',  ( -3.863846776457871776E-17, -0.3155070326520292845, 0.3018750000000037792 ) ) ;
#23970 = CARTESIAN_POINT ( 'NONE',  ( -0.2819296736111110424, 5.016055555631420582, -0.1167790944451423119 ) ) ;
#23971 = ORIENTED_EDGE ( 'NONE', *, *, #4587, .F. ) ;
#23972 = CARTESIAN_POINT ( 'NONE',  ( 0.1568395974156406025, -0.4507144935777573913, 0.4251457422752845661 ) ) ;
#23973 = CARTESIAN_POINT ( 'NONE',  ( 0.3613381517857143232, 0.4223214284738860957, 0.000000000000000000 ) ) ;
#23974 = ORIENTED_EDGE ( 'NONE', *, *, #8701, .F. ) ;
#23975 = CARTESIAN_POINT ( 'NONE',  ( -0.1167790944451422702, 0.3444444443685777402, -0.2819296736111110979 ) ) ;
#23976 = CARTESIAN_POINT ( 'NONE',  ( -0.1144950937579609918, -0.2764156081756484196, 0.2168055555555584712 ) ) ;
#23977 = CARTESIAN_POINT ( 'NONE',  ( -0.2819296736111110979, 4.922305555631420582, 0.000000000000000000 ) ) ;
#23978 = CARTESIAN_POINT ( 'NONE',  ( 0.3051180496388954388, 4.472561363414810032, 0.06516940886235408903 ) ) ;
#23979 = VERTEX_POINT ( 'NONE', #5502 ) ;
#23980 = CARTESIAN_POINT ( 'NONE',  ( -0.1167790944451423257, 4.898000000075866112, -0.2819296736111110424 ) ) ;
#23981 = CARTESIAN_POINT ( 'NONE',  ( -0.1568318157528670875, 4.159500745689967971, -0.2727933530271318130 ) ) ;
#23982 = CARTESIAN_POINT ( 'NONE',  ( 1.020000000000000018, 0.05000000000000028727, -2.591000000000000192 ) ) ;
#23983 = APPROVAL_PERSON_ORGANIZATION ( #14540, #8209, #6977 ) ;
#23984 = CARTESIAN_POINT ( 'NONE',  ( 0.1292346314604031765, 4.088972222222221120, -0.3120000000000024420 ) ) ;
#23985 = CARTESIAN_POINT ( 'NONE',  ( 1.910449006669871087E-17, 0.5874999999999996891, -0.3119999999999999996 ) ) ;
#23986 = CARTESIAN_POINT ( 'NONE',  ( 0.2206173157302028787, 4.738277777777777366, 0.2206173157302027954 ) ) ;
#23987 = CARTESIAN_POINT ( 'NONE',  ( 0.2819296736111110979, 4.047305555631421470, -3.452642723725051716E-17 ) ) ;
#23988 = CARTESIAN_POINT ( 'NONE',  ( 1.910449006669871087E-17, 0.1986111111111107386, -0.3119999999999999996 ) ) ;
#23989 = CARTESIAN_POINT ( 'NONE',  ( 0.1819161012131308708, 4.021594027790507120, 0.2535283937084970574 ) ) ;
#23990 = CARTESIAN_POINT ( 'NONE',  ( 0.01172578639833042440, 0.5344959914317364280, 0.04874733047934381308 ) ) ;
#23991 = ORIENTED_EDGE ( 'NONE', *, *, #17962, .T. ) ;
#23992 = VECTOR ( 'NONE', #8444, 39.37007874015748143 ) ;
#23993 = CARTESIAN_POINT ( 'NONE',  ( -2.266361716303445225E-16, 4.432722222374099630, -0.3119999999999999996 ) ) ;
#23994 = CARTESIAN_POINT ( 'NONE',  ( 0.000000000000000000, 0.4197679491924312112, -0.2501339745962155581 ) ) ;
#23995 = CARTESIAN_POINT ( 'NONE',  ( 0.4687500000000003886, 0.2922835737772483400, 0.06112444011295369017 ) ) ;
#23996 = EDGE_CURVE ( 'NONE', #3037, #13969, #6199, .T. ) ;
#23997 = CARTESIAN_POINT ( 'NONE',  ( -0.1144950937579609918, -0.2764156081756484196, 0.1543055555555579716 ) ) ;
#23998 = DIRECTION ( 'NONE',  ( 0.000000000000000000, 0.000000000000000000, -1.000000000000000000 ) ) ;
#23999 = CARTESIAN_POINT ( 'NONE',  ( -0.1005340957006147506, 4.435645067432016475, -0.2960640309988838981 ) ) ;
#24000 = CARTESIAN_POINT ( 'NONE',  ( -0.2764156081756484196, 0.1144950937579609918, 0.3695833333333373716 ) ) ;
#24001 = CARTESIAN_POINT ( 'NONE',  ( -6.979263641208234666E-17, 0.2080357141881717942, 0.3799334167787516425 ) ) ;
#24002 = CARTESIAN_POINT ( 'NONE',  ( -0.1167790944451422702, 0.2749999999241333204, -0.2819296736111110424 ) ) ;
#24003 = CARTESIAN_POINT ( 'NONE',  ( 0.0003178160707640876313, 3.877158127254288544, -0.3119998483270248202 ) ) ;
#24004 = LINE ( 'NONE', #7316, #20524 ) ;
#24005 = CC_DESIGN_PERSON_AND_ORGANIZATION_ASSIGNMENT ( #19297, #2603, ( #9980 ) ) ;
#24006 = CYLINDRICAL_SURFACE ( 'NONE', #8977, 0.3119999999999999996 ) ;
#24007 = CARTESIAN_POINT ( 'NONE',  ( 0.2764156081756483641, -0.1144950937579611167, 0.008472222222223456389 ) ) ;
#24008 = EDGE_CURVE ( 'NONE', #18353, #11483, #18548, .T. ) ;
#24009 = ORIENTED_EDGE ( 'NONE', *, *, #4739, .T. ) ;
#24010 = ORIENTED_EDGE ( 'NONE', *, *, #23741, .T. ) ;
#24011 = CARTESIAN_POINT ( 'NONE',  ( -0.04071097728432398338, 5.093190941573745967, -0.3088414402879665066 ) ) ;
#24012 = CARTESIAN_POINT ( 'NONE',  ( 0.4591128671207585499, 0.1125912384831261187, 0.4269528428895272287 ) ) ;
#24013 = CARTESIAN_POINT ( 'NONE',  ( -5.731347020009612645E-17, 0.004166666666666329205, 0.3119999999999999996 ) ) ;
#24014 = CARTESIAN_POINT ( 'NONE',  ( 0.2819296736111110979, 3.779944444520310309, 0.1167790944451422425 ) ) ;
#24015 = CARTESIAN_POINT ( 'NONE',  ( 0.3613381517857143232, 0.1508928570453147155, 0.1174058825155742114 ) ) ;
#24016 = CARTESIAN_POINT ( 'NONE',  ( 0.1167790944451422702, 4.460500000075867000, -0.2819296736111110424 ) ) ;
#24017 = CARTESIAN_POINT ( 'NONE',  ( 0.3119999999999999996, 4.970916666666665762, -0.1292346314604056745 ) ) ;
#24018 = PLANE ( 'NONE',  #21163 ) ;
#24019 = ORIENTED_EDGE ( 'NONE', *, *, #16789, .T. ) ;
#24020 = CARTESIAN_POINT ( 'NONE',  ( 0.08156453417730161193, 4.351642364793766760, 0.3038997693205980899 ) ) ;
#24021 = CARTESIAN_POINT ( 'NONE',  ( 0.1167790944451424368, 5.036888888964754507, 0.2819296736111110424 ) ) ;
#24022 = CARTESIAN_POINT ( 'NONE',  ( -0.04912707777265164222, 5.144593440471582291, -0.2998369709411419781 ) ) ;
#24023 = AXIS2_PLACEMENT_3D ( 'NONE', #15941, #23244, #23367 ) ;
#24024 = CARTESIAN_POINT ( 'NONE',  ( -0.4749999999999999778, 3.700000000000000622, -0.09499999999999995948 ) ) ;
#24025 = LINE ( 'NONE', #5745, #9921 ) ;
#24026 = CARTESIAN_POINT ( 'NONE',  ( 0.2819296736111110979, 4.658416666742532186, -3.452642723725051716E-17 ) ) ;
#24027 = PERSON_AND_ORGANIZATION_ROLE ( 'classification_officer' ) ;
#24028 = CARTESIAN_POINT ( 'NONE',  ( 0.000000000000000000, 0.05000000000000028727, 0.000000000000000000 ) ) ;
#24029 = CARTESIAN_POINT ( 'NONE',  ( -0.1292346314604056190, 0.4173611109593781676, -0.3119999999999999996 ) ) ;
#24030 = CARTESIAN_POINT ( 'NONE',  ( -0.2819296736111110424, 0.4624999999241333759, -0.1167790944451423396 ) ) ;
#24031 = ORIENTED_EDGE ( 'NONE', *, *, #23423, .F. ) ;
#24032 = VERTEX_POINT ( 'NONE', #15021 ) ;
#24033 = CARTESIAN_POINT ( 'NONE',  ( -0.1167790944451422702, 0.1777777777019111383, -0.2819296736111110424 ) ) ;
#24034 = LINE ( 'NONE', #16851, #15463 ) ;
#24035 = LINE ( 'NONE', #10775, #11321 ) ;
#24036 = CARTESIAN_POINT ( 'NONE',  ( 0.3236067977499790249, -0.09285714285714286031, -0.2351141009169892826 ) ) ;
#24037 = CARTESIAN_POINT ( 'NONE',  ( -0.1306872919485614903, 0.3155070326520293400, -0.1147916666666666252 ) ) ;
#24038 = EDGE_CURVE ( 'NONE', #5917, #314, #4793, .T. ) ;
#24039 = CARTESIAN_POINT ( 'NONE',  ( 0.4687500000000002776, -0.2172771893995191772, 0.3896678519206923097 ) ) ;
#24040 = CARTESIAN_POINT ( 'NONE',  ( -0.05856351884197068952, 3.878803041371024385, -0.3066960576329920696 ) ) ;
#24041 = CARTESIAN_POINT ( 'NONE',  ( 1.108892417209500936, 2.340112590966282546, -1.018235385338814192 ) ) ;
#24042 = CARTESIAN_POINT ( 'NONE',  ( 0.2819296736111110424, 4.509111111186976828, -0.1167790944451423396 ) ) ;
#24043 = AXIS2_PLACEMENT_3D ( 'NONE', #23650, #5124, #12590 ) ;
#24044 = CARTESIAN_POINT ( 'NONE',  ( 0.4000000000000000222, 0.1053571426620580620, 0.000000000000000000 ) ) ;
#24045 = CARTESIAN_POINT ( 'NONE',  ( -0.3120000000000000551, 0.2645833331816004330, 0.1292346314604056190 ) ) ;
#24046 = CARTESIAN_POINT ( 'NONE',  ( 0.2819296736111110979, 5.172305555631421470, -3.452642723725051716E-17 ) ) ;
#24047 = CARTESIAN_POINT ( 'NONE',  ( -0.1167790944451423535, 4.363277777853642903, 0.2819296736111110979 ) ) ;
#24048 = CARTESIAN_POINT ( 'NONE',  ( 0.04921115518204333128, 3.764677272939175090, -0.3083034729010514785 ) ) ;
#24049 = PLANE ( 'NONE',  #23386 ) ;
#24050 = CARTESIAN_POINT ( 'NONE',  ( 0.000000000000000000, 0.000000000000000000, 0.000000000000000000 ) ) ;
#24051 = CARTESIAN_POINT ( 'NONE',  ( 0.1292346314604056190, 4.151472222373953969, -0.3119999999999999996 ) ) ;
#24052 = CARTESIAN_POINT ( 'NONE',  ( 0.2819296736111110979, 4.450083333409199149, -3.452642723725051716E-17 ) ) ;
#24053 = CARTESIAN_POINT ( 'NONE',  ( 0.1993543840281266633, 3.887583333409198705, -0.1993543840281266910 ) ) ;
#24054 = EDGE_LOOP ( 'NONE', ( #9097, #12708, #17496, #13538 ) ) ;
#24055 = EDGE_CURVE ( 'NONE', #1317, #2053, #1871, .T. ) ;
#24056 = VECTOR ( 'NONE', #19567, 39.37007874015748143 ) ;
#24057 = ORIENTED_EDGE ( 'NONE', *, *, #13258, .T. ) ;
#24058 = APPROVAL_STATUS ( 'not_yet_approved' ) ;
#24059 = CARTESIAN_POINT ( 'NONE',  ( 0.04581704741080250276, -0.3043534538584632965, 0.4189930025942082414 ) ) ;
#24060 = LINE ( 'NONE', #23572, #4862 ) ;
#24061 = DIRECTION ( 'NONE',  ( -0.000000000000000000, -1.000000000000000000, -0.000000000000000000 ) ) ;
#24062 = VERTEX_POINT ( 'NONE', #15166 ) ;
#24063 = CARTESIAN_POINT ( 'NONE',  ( -0.1292346314604058410, 0.5493055554038226429, 0.3119999999999998885 ) ) ;
#24064 = CARTESIAN_POINT ( 'NONE',  ( 0.3125000000000000555, -5.740531871003217465E-17, 0.2063888888888918416 ) ) ;
#24065 = CARTESIAN_POINT ( 'NONE',  ( 2.986000000000000210, 2.690000000000002167, -0.07500000000000014988 ) ) ;
#24066 = CARTESIAN_POINT ( 'NONE',  ( 0.3613381517857143232, -0.07767857152611380711, 0.000000000000000000 ) ) ;
#24067 = CARTESIAN_POINT ( 'NONE',  ( -0.2206173157302028787, 0.4972222222222218435, 0.2206173157302027954 ) ) ;
#24068 = EDGE_CURVE ( 'NONE', #20092, #21184, #16120, .T. ) ;
#24069 = ORIENTED_EDGE ( 'NONE', *, *, #940, .T. ) ;
#24070 = ORIENTED_EDGE ( 'NONE', *, *, #12849, .F. ) ;
#24071 = CARTESIAN_POINT ( 'NONE',  ( -0.3613381517857143788, 0.05089285704531475163, 0.1174058825155740310 ) ) ;
#24072 = ORIENTED_EDGE ( 'NONE', *, *, #23811, .F. ) ;
#24073 = CARTESIAN_POINT ( 'NONE',  ( 0.07683745418995416299, 5.097786225156845319, -0.3020026545442724419 ) ) ;
#24074 = CARTESIAN_POINT ( 'NONE',  ( 0.1954553509668047195, 0.1954553509668046085, 0.3452777777777817358 ) ) ;
#24075 = CARTESIAN_POINT ( 'NONE',  ( 0.2819296736111110979, 4.266055555631421470, 0.1167790944451422425 ) ) ;
#24076 = CARTESIAN_POINT ( 'NONE',  ( -0.1993543840281266910, 5.068138888964754507, -0.1993543840281266910 ) ) ;
#24077 =( BOUNDED_CURVE ( )  B_SPLINE_CURVE ( 2, ( #10395, #15630, #19402, #12111, #17695, #15509, #11866, #23163, #4756 ),
 .UNSPECIFIED., .F., .F. ) 
 B_SPLINE_CURVE_WITH_KNOTS ( ( 3, 2, 2, 2, 3 ),
 ( 0.7291666666666666297, 0.7395833333333333703, 0.7500000000000000000, 0.7604166666666666297, 0.7708333333333333703 ),
 .UNSPECIFIED. ) 
 CURVE ( )  GEOMETRIC_REPRESENTATION_ITEM ( )  RATIONAL_B_SPLINE_CURVE ( ( 1.000000000000000000, 0.9238795325112867385, 1.000000000000000000, 0.9238795325112867385, 1.000000000000000000, 0.9238795325112867385, 1.000000000000000000, 0.9238795325112867385, 1.000000000000000000 ) ) 
 REPRESENTATION_ITEM ( '' )  );
#24078 = CARTESIAN_POINT ( 'NONE',  ( -0.4687500000000004441, 0.04389001238043890862, 0.09139217099949115131 ) ) ;
#24079 = CARTESIAN_POINT ( 'NONE',  ( -0.1292346314604056190, 0.3618055554038226429, -0.3119999999999999996 ) ) ;
#24080 = CARTESIAN_POINT ( 'NONE',  ( -0.1292346314604056745, 3.873694444444442997, -0.3119999999999999996 ) ) ;
#24081 = AXIS2_PLACEMENT_3D ( 'NONE', #1258, #6504, #23551 ) ;
#24082 = CARTESIAN_POINT ( 'NONE',  ( -0.2206173157302028232, 4.884111111262843252, -0.2206173157302028232 ) ) ;
#24083 = CARTESIAN_POINT ( 'NONE',  ( 0.3107418214344630503, 4.806955620829070241, 0.02800764279169619744 ) ) ;
#24084 = EDGE_CURVE ( 'NONE', #10770, #8566, #20644, .T. ) ;
#24085 = CARTESIAN_POINT ( 'NONE',  ( 0.3119999999999999996, 4.856333333333332725, -3.820898013339742174E-17 ) ) ;
#24086 = ORIENTED_EDGE ( 'NONE', *, *, #10077, .T. ) ;
#24087 = CARTESIAN_POINT ( 'NONE',  ( 0.2461656082887962727, 0.03739867468129062789, -0.1491120642768181681 ) ) ;
#24088 = ORIENTED_EDGE ( 'NONE', *, *, #1309, .F. ) ;
#24089 = CARTESIAN_POINT ( 'NONE',  ( -0.3155070326520293400, -0.1306872919485614626, 0.2914583333333370385 ) ) ;
#24090 = CARTESIAN_POINT ( 'NONE',  ( 0.1167790944451422702, 5.113277777853642903, -0.2819296736111110424 ) ) ;
#24091 = VECTOR ( 'NONE', #18753, 39.37007874015748143 ) ;
#24092 = ORIENTED_EDGE ( 'NONE', *, *, #2915, .F. ) ;
#24093 = CARTESIAN_POINT ( 'NONE',  ( 0.1517119284478177232, -0.4426845032613774267, 0.4305326508994914425 ) ) ;
#24094 = EDGE_CURVE ( 'NONE', #606, #4893, #15283, .T. ) ;
#24095 = CARTESIAN_POINT ( 'NONE',  ( 2.326421213736078119E-17, 0.3687499999024574371, -0.3799334167787516425 ) ) ;
#24096 = VERTEX_POINT ( 'NONE', #401 ) ;
#24097 = CARTESIAN_POINT ( 'NONE',  ( -0.1167790944451422702, 0.2888888888130222710, -0.2819296736111110979 ) ) ;
#24098 = CARTESIAN_POINT ( 'NONE',  ( -0.2764156081756484196, 1.692557448933383907E-17, 0.1508333333333356785 ) ) ;
#24099 = CARTESIAN_POINT ( 'NONE',  ( 0.1167790944451424368, 4.884111111186977716, 0.2819296736111110424 ) ) ;
#24100 = CARTESIAN_POINT ( 'NONE',  ( -0.1698811246235177597, 3.066692553488282957, 3.107674353005361212 ) ) ;
#24101 = CARTESIAN_POINT ( 'NONE',  ( -0.2819296736111110424, 4.904944444520310753, -0.1167790944451423119 ) ) ;
#24102 = CARTESIAN_POINT ( 'NONE',  ( -0.06335377612981449302, 0.05361622414587396968, -0.4000000000000000222 ) ) ;
#24103 = CARTESIAN_POINT ( 'NONE',  ( -0.2206173157302027676, 5.057722222222222008, 0.2206173157302028787 ) ) ;
#24104 = CARTESIAN_POINT ( 'NONE',  ( 1.573500000000000343, 2.683750000000000746, -1.412500000000000089 ) ) ;
#24105 = CARTESIAN_POINT ( 'NONE',  ( 1.908027509798675192, 2.439495096761425508, -1.906576846642106027 ) ) ;
#24106 = CARTESIAN_POINT ( 'NONE',  ( -0.3119999999999999996, 4.606333333333332725, 0.000000000000000000 ) ) ;
#24107 = CARTESIAN_POINT ( 'NONE',  ( -0.1167790944451423535, 3.974388888964754063, 0.2819296736111110979 ) ) ;
#24108 = CARTESIAN_POINT ( 'NONE',  ( 1.910449006669871087E-17, 0.1430555555555552139, -0.3119999999999999996 ) ) ;
#24109 = CARTESIAN_POINT ( 'NONE',  ( 0.2954588070498663788, 4.032821911431771156, -0.1002473225235935156 ) ) ;
#24110 = CARTESIAN_POINT ( 'NONE',  ( 0.3119999999999999996, 4.415361111111110404, -0.1292346314604056745 ) ) ;
#24111 = VECTOR ( 'NONE', #10131, 39.37007874015748854 ) ;
#24112 = ORIENTED_EDGE ( 'NONE', *, *, #23687, .F. ) ;
#24113 = CARTESIAN_POINT ( 'NONE',  ( -0.1724646555813178495, 4.121954259501087847, 0.2600007236767823415 ) ) ;
#24114 = CARTESIAN_POINT ( 'NONE',  ( 0.02148743539037334394, 4.654328078246623868, -0.3113644187995892598 ) ) ;
#24115 = CARTESIAN_POINT ( 'NONE',  ( 0.1144950937579611444, 0.2764156081756483641, 0.1820833333333359561 ) ) ;
#24116 = DIRECTION ( 'NONE',  ( -0.000000000000000000, -0.000000000000000000, -1.000000000000000000 ) ) ;
#24117 = ADVANCED_FACE ( 'NONE', ( #6123 ), #279, .F. ) ;
#24118 = CARTESIAN_POINT ( 'NONE',  ( -0.2233192592356399442, 0.3223214284738860624, -0.3073725909049500049 ) ) ;
#24119 = CARTESIAN_POINT ( 'NONE',  ( 0.1993543840281266355, 0.1951388888130222155, 0.1993543840281267465 ) ) ;
#24120 = CARTESIAN_POINT ( 'NONE',  ( 0.4687500000000002776, -0.1743509873645021913, 0.07807871097225772827 ) ) ;
#24121 = CARTESIAN_POINT ( 'NONE',  ( 0.1292346314604056745, 0.5840277777777772572, -0.3119999999999999996 ) ) ;
#24122 = CARTESIAN_POINT ( 'NONE',  ( -0.3385998376278290256, 3.738758431839877614E-19, -0.1199999999999999956 ) ) ;
#24123 = CARTESIAN_POINT ( 'NONE',  ( -0.1954553509668046918, -0.1954553509668046640, -0.008888888888887799475 ) ) ;
#24124 = CARTESIAN_POINT ( 'NONE',  ( -0.1376149012345692091, 5.096011253522892304, -0.2798126666846854627 ) ) ;
#24125 = CARTESIAN_POINT ( 'NONE',  ( 0.4687500000000002220, -0.08887898168693945944, 0.4252295499841368120 ) ) ;
#24126 = CARTESIAN_POINT ( 'NONE',  ( -0.3119999999999999996, 0.04236111111111078020, -0.1292346314604056745 ) ) ;
#24127 = CARTESIAN_POINT ( 'NONE',  ( 0.2206173157302027954, 5.252166666666665762, -0.2206173157302028232 ) ) ;
#24128 = AXIS2_PLACEMENT_3D ( 'NONE', #5727, #12948, #13186 ) ;
#24129 = NEXT_ASSEMBLY_USAGE_OCCURRENCE ( 'NAUO1', ' ', ' ', #6872, #21185, $ ) ;
#24130 = NEXT_ASSEMBLY_USAGE_OCCURRENCE ( 'NAUO2', ' ', ' ', #6872, #15678, $ ) ;
#24131 = NEXT_ASSEMBLY_USAGE_OCCURRENCE ( 'NAUO3', ' ', ' ', #6872, #2989, $ ) ;
#24132 = NEXT_ASSEMBLY_USAGE_OCCURRENCE ( 'NAUO4', ' ', ' ', #6872, #13174, $ ) ;
#24133 = NEXT_ASSEMBLY_USAGE_OCCURRENCE ( 'NAUO5', ' ', ' ', #6872, #19252, $ ) ;
#24134 = NEXT_ASSEMBLY_USAGE_OCCURRENCE ( 'NAUO6', ' ', ' ', #6872, #8791, $ ) ;
#24135 = NEXT_ASSEMBLY_USAGE_OCCURRENCE ( 'NAUO7', ' ', ' ', #6872, #10901, $ ) ;
#24136 = NEXT_ASSEMBLY_USAGE_OCCURRENCE ( 'NAUO8', ' ', ' ', #6872, #9710, $ ) ;
#24137 = NEXT_ASSEMBLY_USAGE_OCCURRENCE ( 'NAUO9', ' ', ' ', #6872, #14477, $ ) ;
#24138 = COLOUR_RGB('Deep Blue', 0.66274510, 0.83137255, 0.94901961);
#24139 = FILL_AREA_STYLE_COLOUR('',#24138);
#24140 = FILL_AREA_STYLE('',(#24139));
#24141 = SURFACE_STYLE_FILL_AREA(#24140);
#24142 = SURFACE_SIDE_STYLE('',(#24141));
#24143 = SURFACE_STYLE_USAGE(.BOTH.,#24142);
#24144 = PRESENTATION_STYLE_ASSIGNMENT((#24143));
#24145 = COLOUR_RGB('Light Blue', 0.31764706, 0.68627451, 0.89019608);
#24146 = FILL_AREA_STYLE_COLOUR('',#24145);
#24147 = FILL_AREA_STYLE('',(#24146));
#24148 = SURFACE_STYLE_FILL_AREA(#24147);
#24149 = SURFACE_SIDE_STYLE('',(#24148));
#24150 = SURFACE_STYLE_USAGE(.BOTH.,#24149);
#24151 = PRESENTATION_STYLE_ASSIGNMENT((#24150));
#24152 = COLOUR_RGB('Sky Blue', 0.40784314, 0.44705882, 0.49803922);
#24153 = FILL_AREA_STYLE_COLOUR('',#24152);
#24154 = FILL_AREA_STYLE('',(#24153));
#24155 = SURFACE_STYLE_FILL_AREA(#24154);
#24156 = SURFACE_SIDE_STYLE('',(#24155));
#24157 = SURFACE_STYLE_USAGE(.BOTH.,#24156);
#24158 = PRESENTATION_STYLE_ASSIGNMENT((#24157));
#24159 = COLOUR_RGB('Slate Gray', 0.72549020, 0.75294118, 0.79215686);
#24160 = FILL_AREA_STYLE_COLOUR('',#24159);
#24161 = FILL_AREA_STYLE('',(#24160));
#24162 = SURFACE_STYLE_FILL_AREA(#24161);
#24163 = SURFACE_SIDE_STYLE('',(#24162));
#24164 = SURFACE_STYLE_USAGE(.BOTH.,#24163);
#24165 = PRESENTATION_STYLE_ASSIGNMENT((#24164));
#24166 = COLOUR_RGB('Light Gray', 0.08235294, 0.09019608, 0.10196078);
#24167 = FILL_AREA_STYLE_COLOUR('',#24166);
#24168 = FILL_AREA_STYLE('',(#24167));
#24169 = SURFACE_STYLE_FILL_AREA(#24168);
#24170 = SURFACE_SIDE_STYLE('',(#24169));
#24171 = SURFACE_STYLE_USAGE(.BOTH.,#24170);
#24172 = PRESENTATION_STYLE_ASSIGNMENT((#24171));
#24173 = COLOUR_RGB('Black', 0.09019608, 0.27058824, 0.51372549);
#24174 = FILL_AREA_STYLE_COLOUR('',#24173);
#24175 = FILL_AREA_STYLE('',(#24174));
#24176 = SURFACE_STYLE_FILL_AREA(#24175);
#24177 = SURFACE_SIDE_STYLE('',(#24176));
#24178 = SURFACE_STYLE_USAGE(.BOTH.,#24177);
#24179 = PRESENTATION_STYLE_ASSIGNMENT((#24178));
#24180 = STYLED_ITEM('',(#24144),#1044);
#24181 = MECHANICAL_DESIGN_GEOMETRIC_PRESENTATION_REPRESENTATION('',(#24180),#5239);
#24182 = STYLED_ITEM('',(#24179),#9145);
#24183 = MECHANICAL_DESIGN_GEOMETRIC_PRESENTATION_REPRESENTATION('',(#24182),#558);
#24184 = STYLED_ITEM('',(#24158),#1208);
#24185 = MECHANICAL_DESIGN_GEOMETRIC_PRESENTATION_REPRESENTATION('',(#24184),#2138);
#24186 = STYLED_ITEM('',(#24172),#8780);
#24187 = MECHANICAL_DESIGN_GEOMETRIC_PRESENTATION_REPRESENTATION('',(#24186),#14988);
#24188 = STYLED_ITEM('',(#24165),#1448);
#24189 = MECHANICAL_DESIGN_GEOMETRIC_PRESENTATION_REPRESENTATION('',(#24188),#15765);
#24190 = STYLED_ITEM('',(#24158),#17608);
#24191 = MECHANICAL_DESIGN_GEOMETRIC_PRESENTATION_REPRESENTATION('',(#24190),#20827);
#24192 = STYLED_ITEM('',(#24144),#17087);
#24193 = MECHANICAL_DESIGN_GEOMETRIC_PRESENTATION_REPRESENTATION('',(#24192),#2886);
#24194 = STYLED_ITEM('',(#24151),#17529);
#24195 = MECHANICAL_DESIGN_GEOMETRIC_PRESENTATION_REPRESENTATION('',(#24194),#12664);
#24196 = STYLED_ITEM('',(#24151),#1082);
#24197 = MECHANICAL_DESIGN_GEOMETRIC_PRESENTATION_REPRESENTATION('',(#24196),#7955);
ENDSEC;
END-ISO-10303-21;
